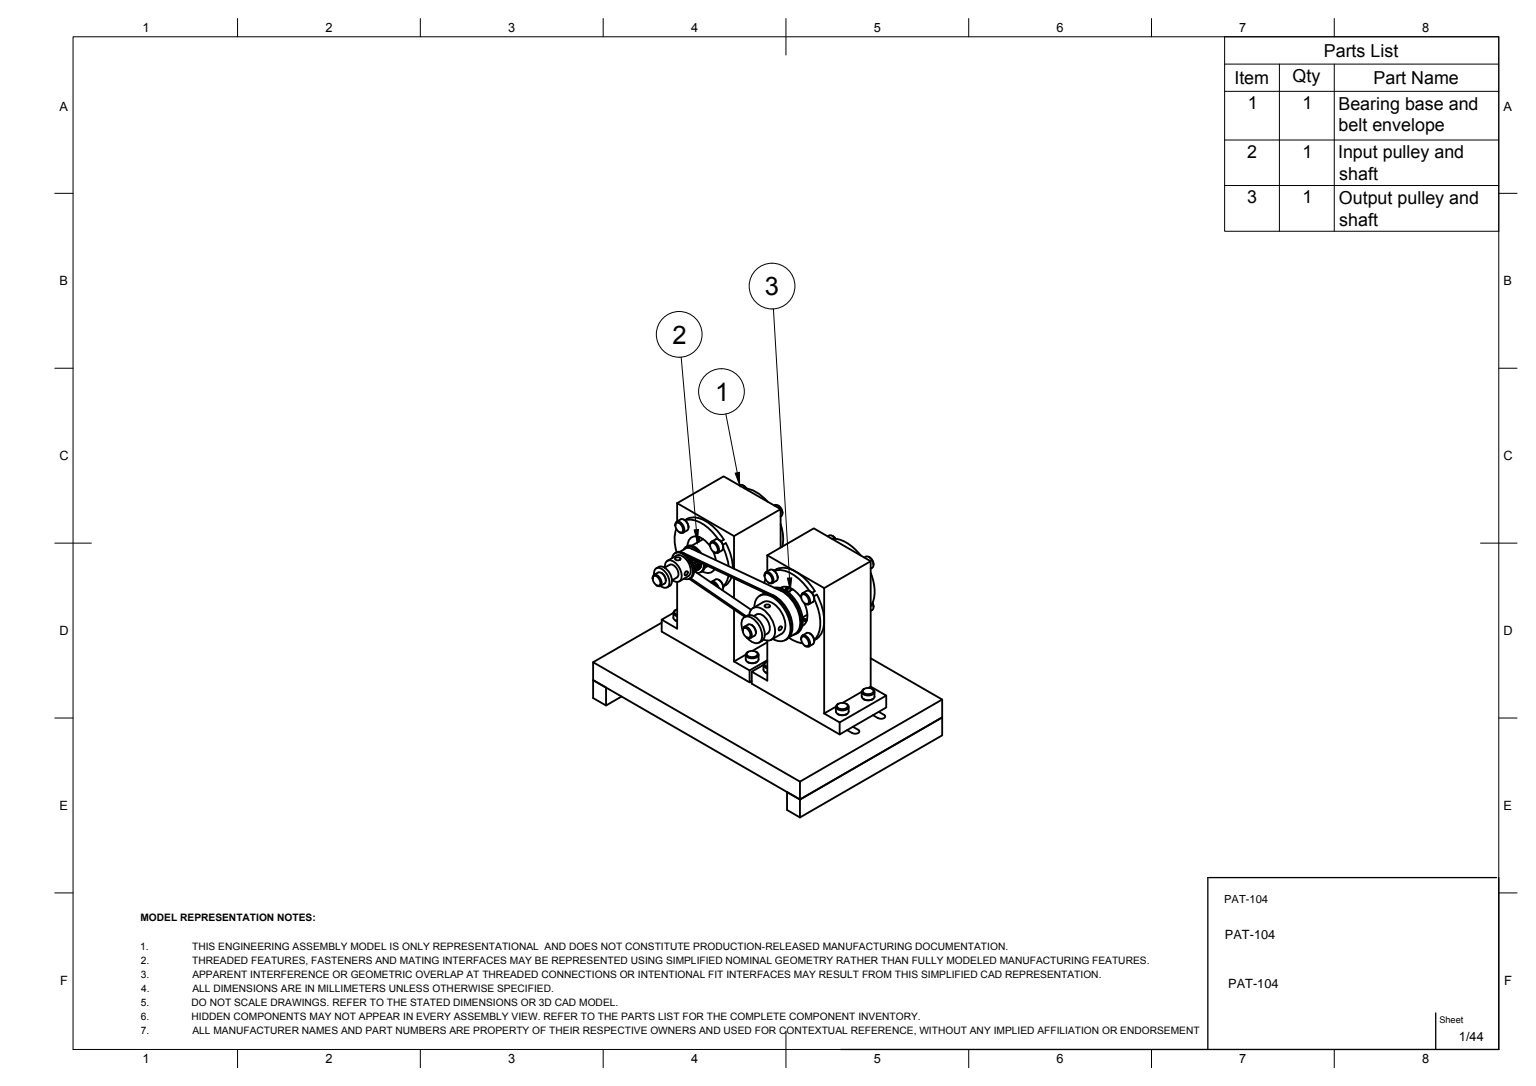
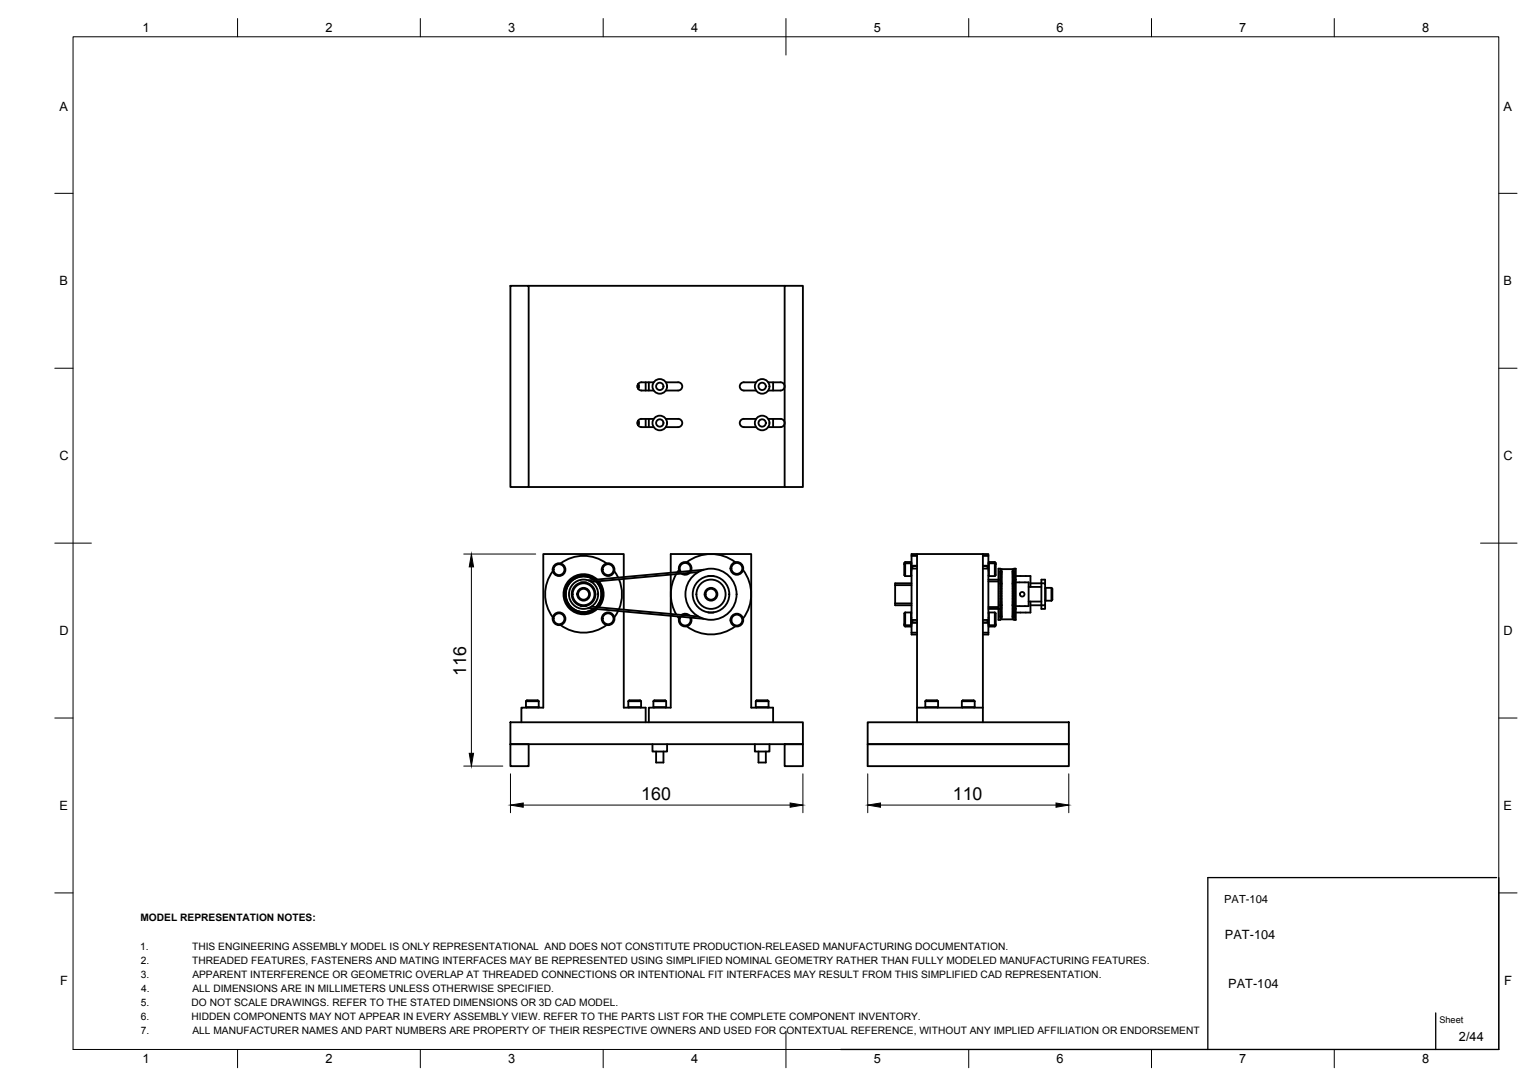
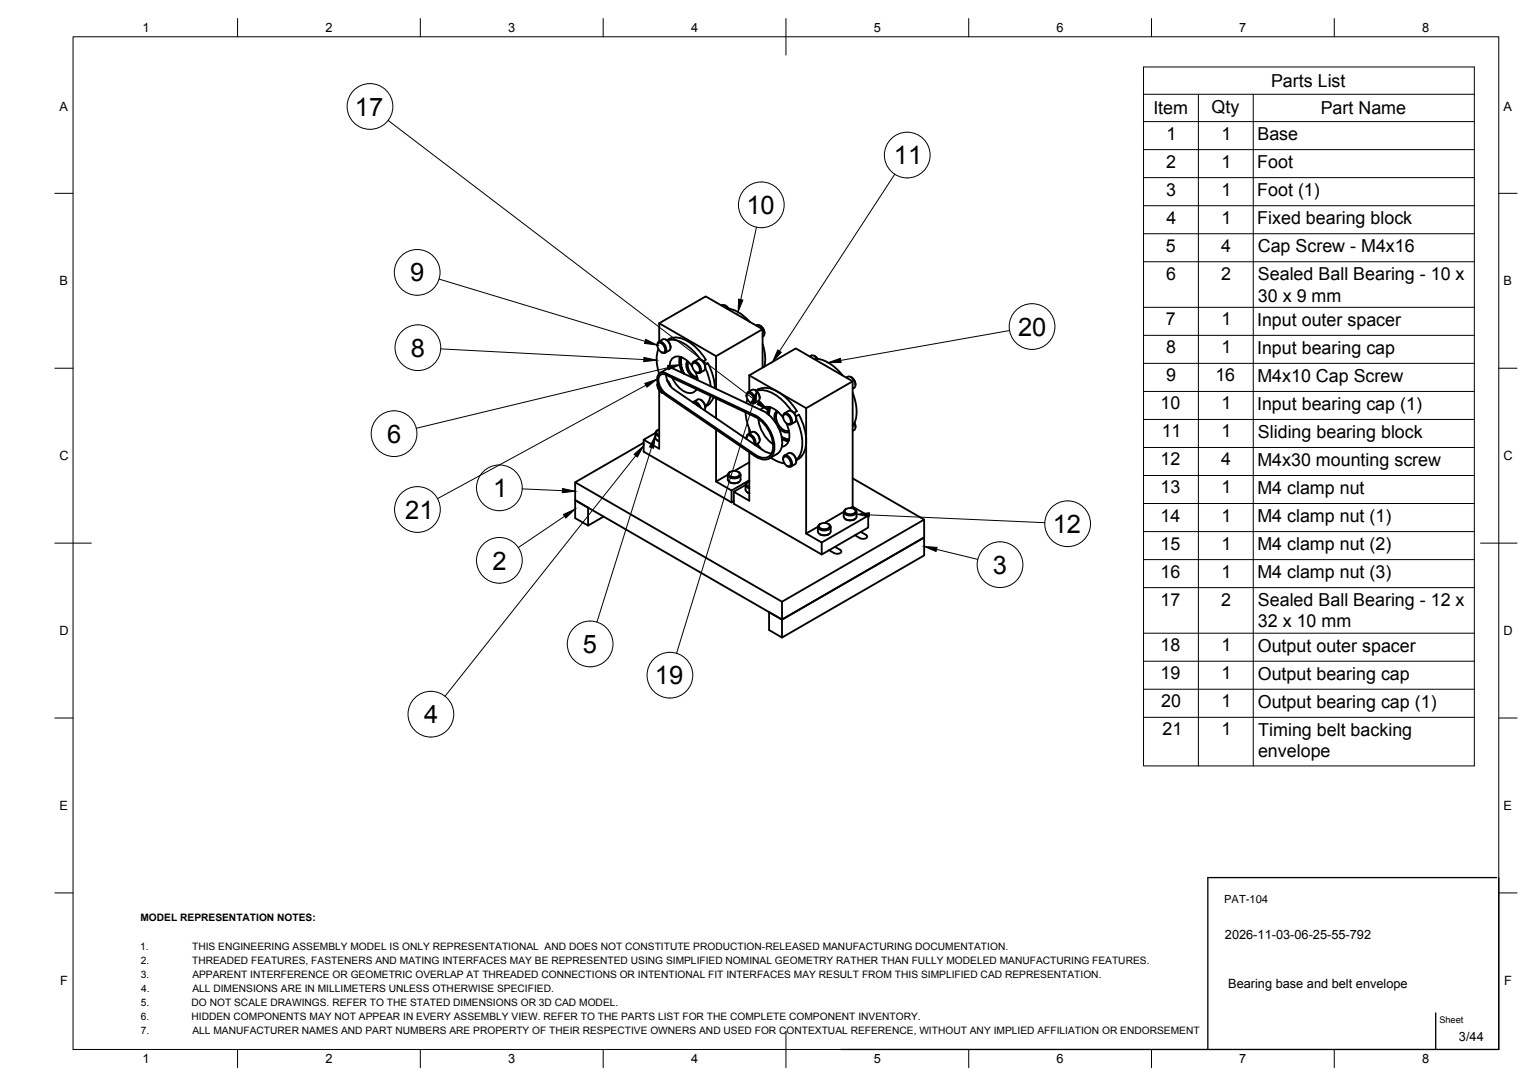
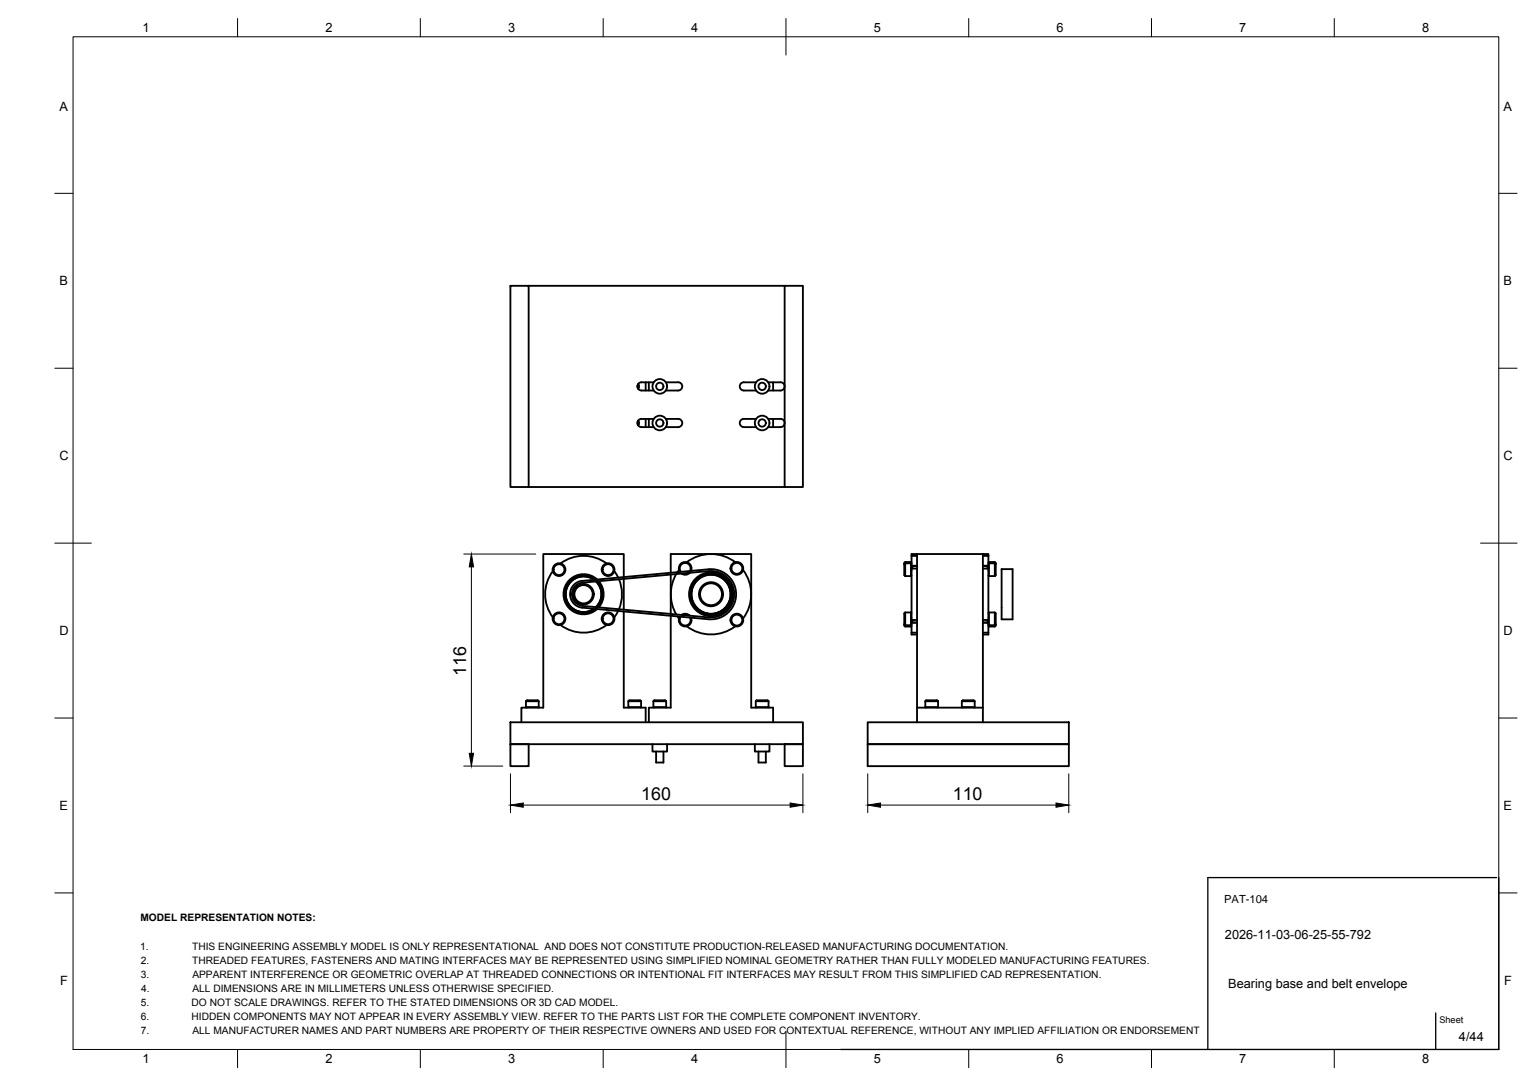
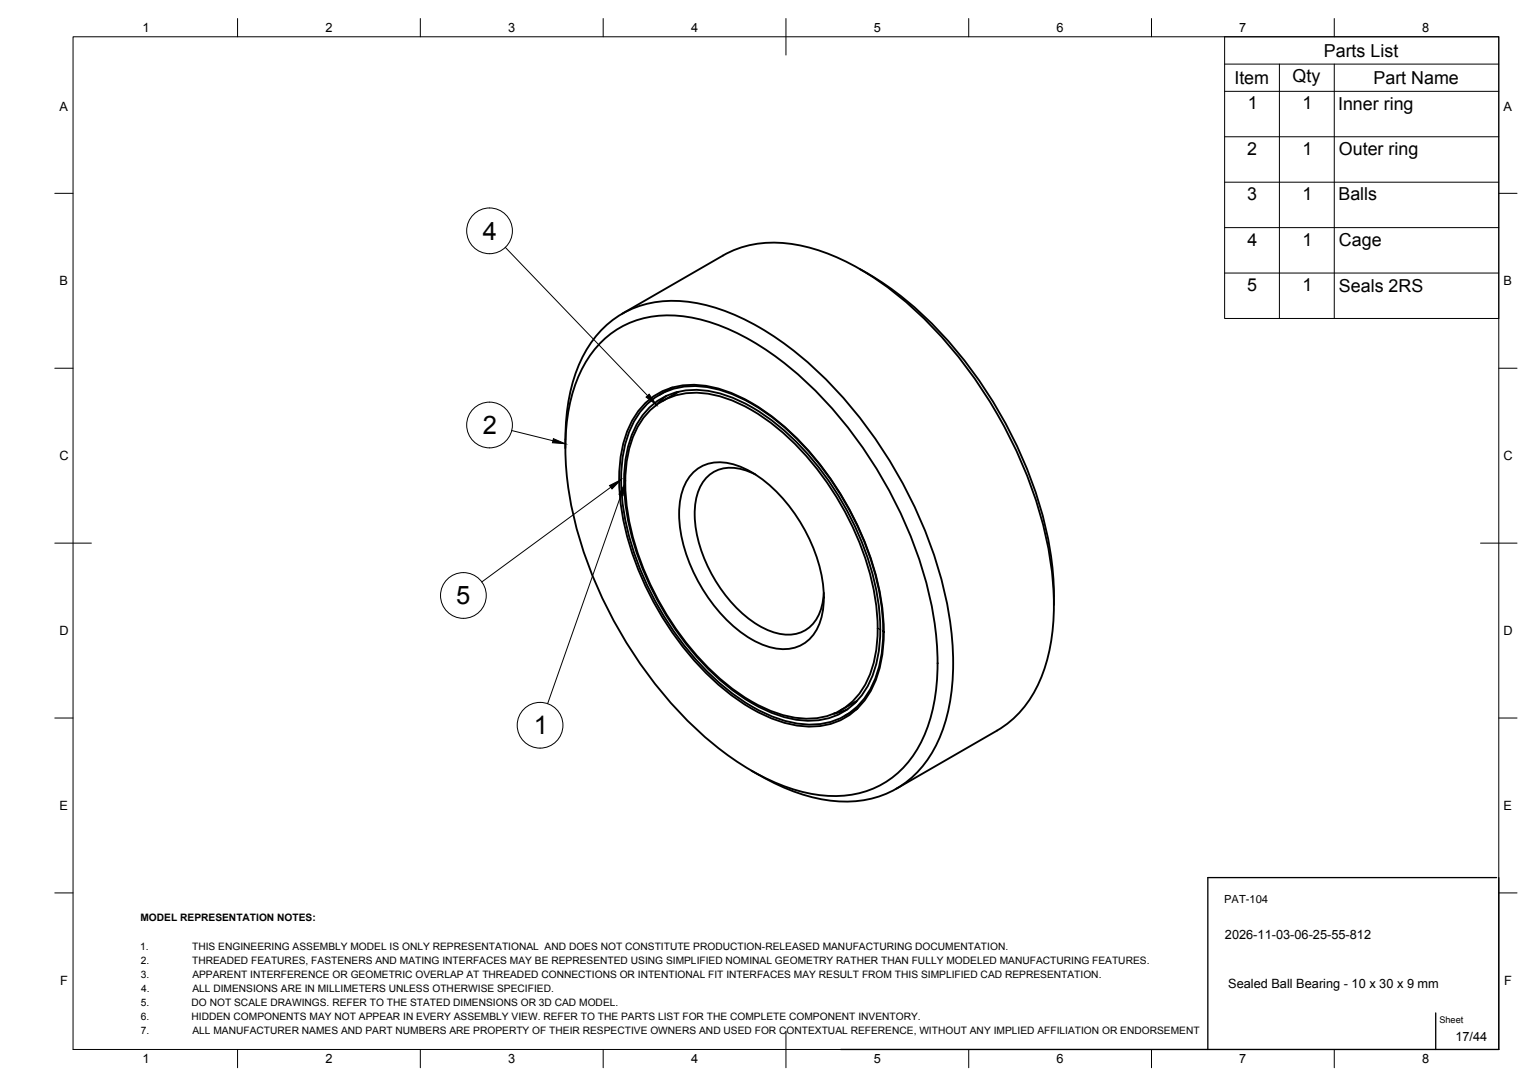
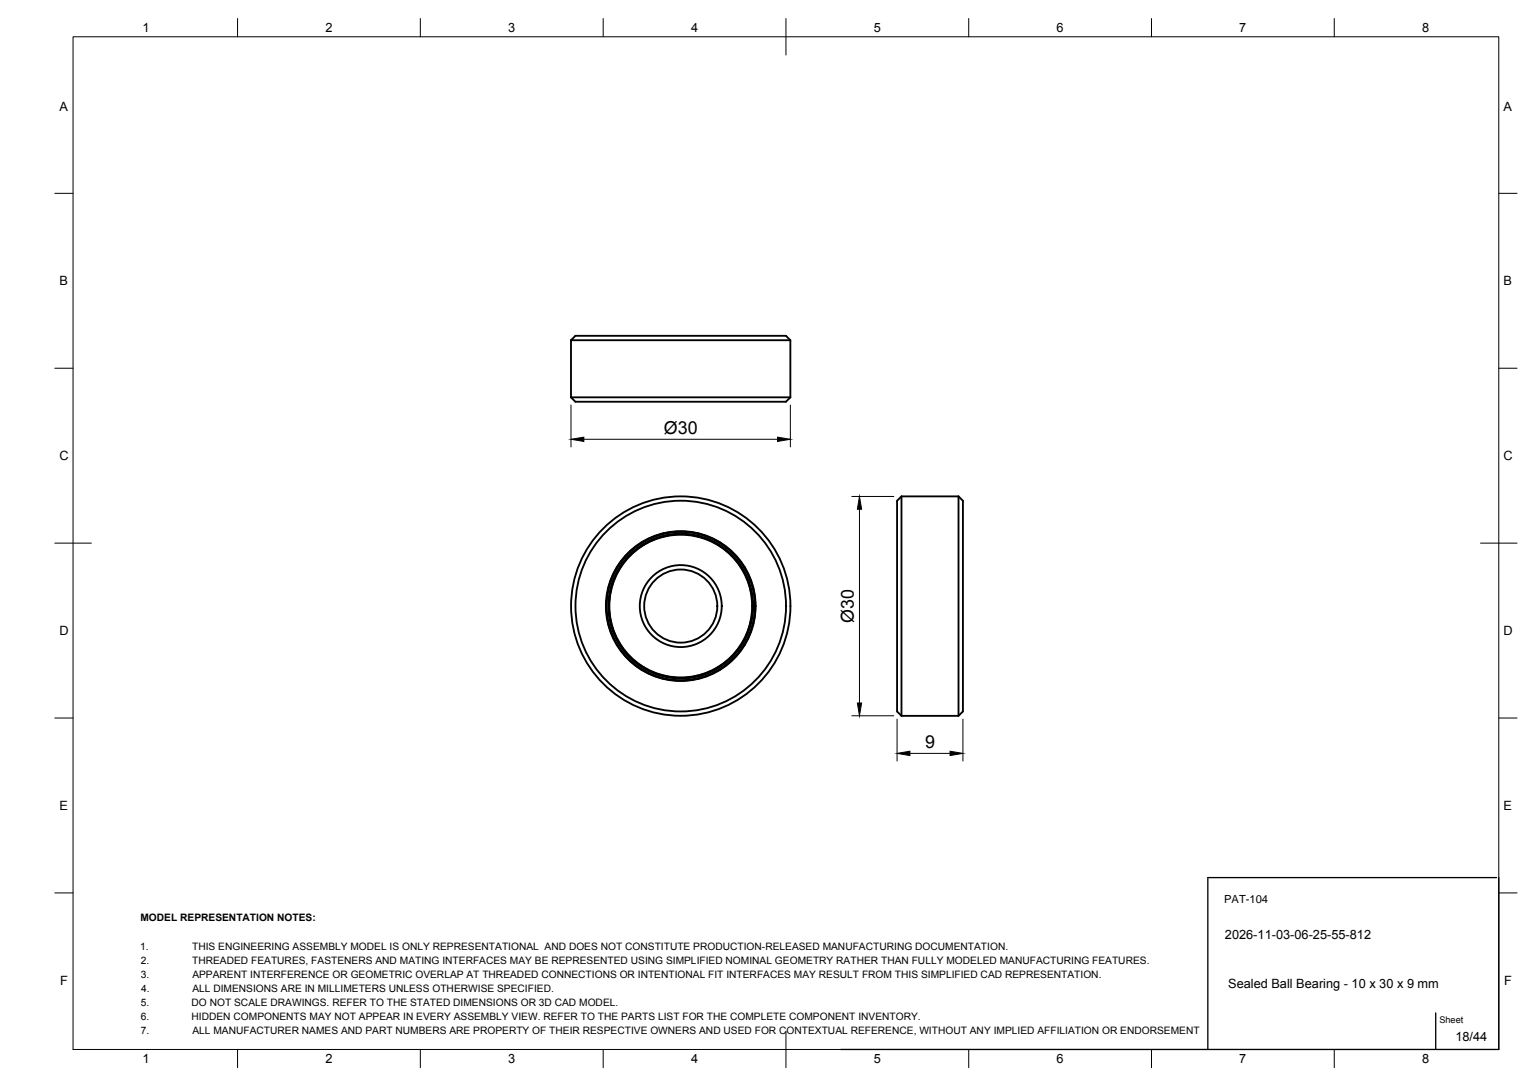
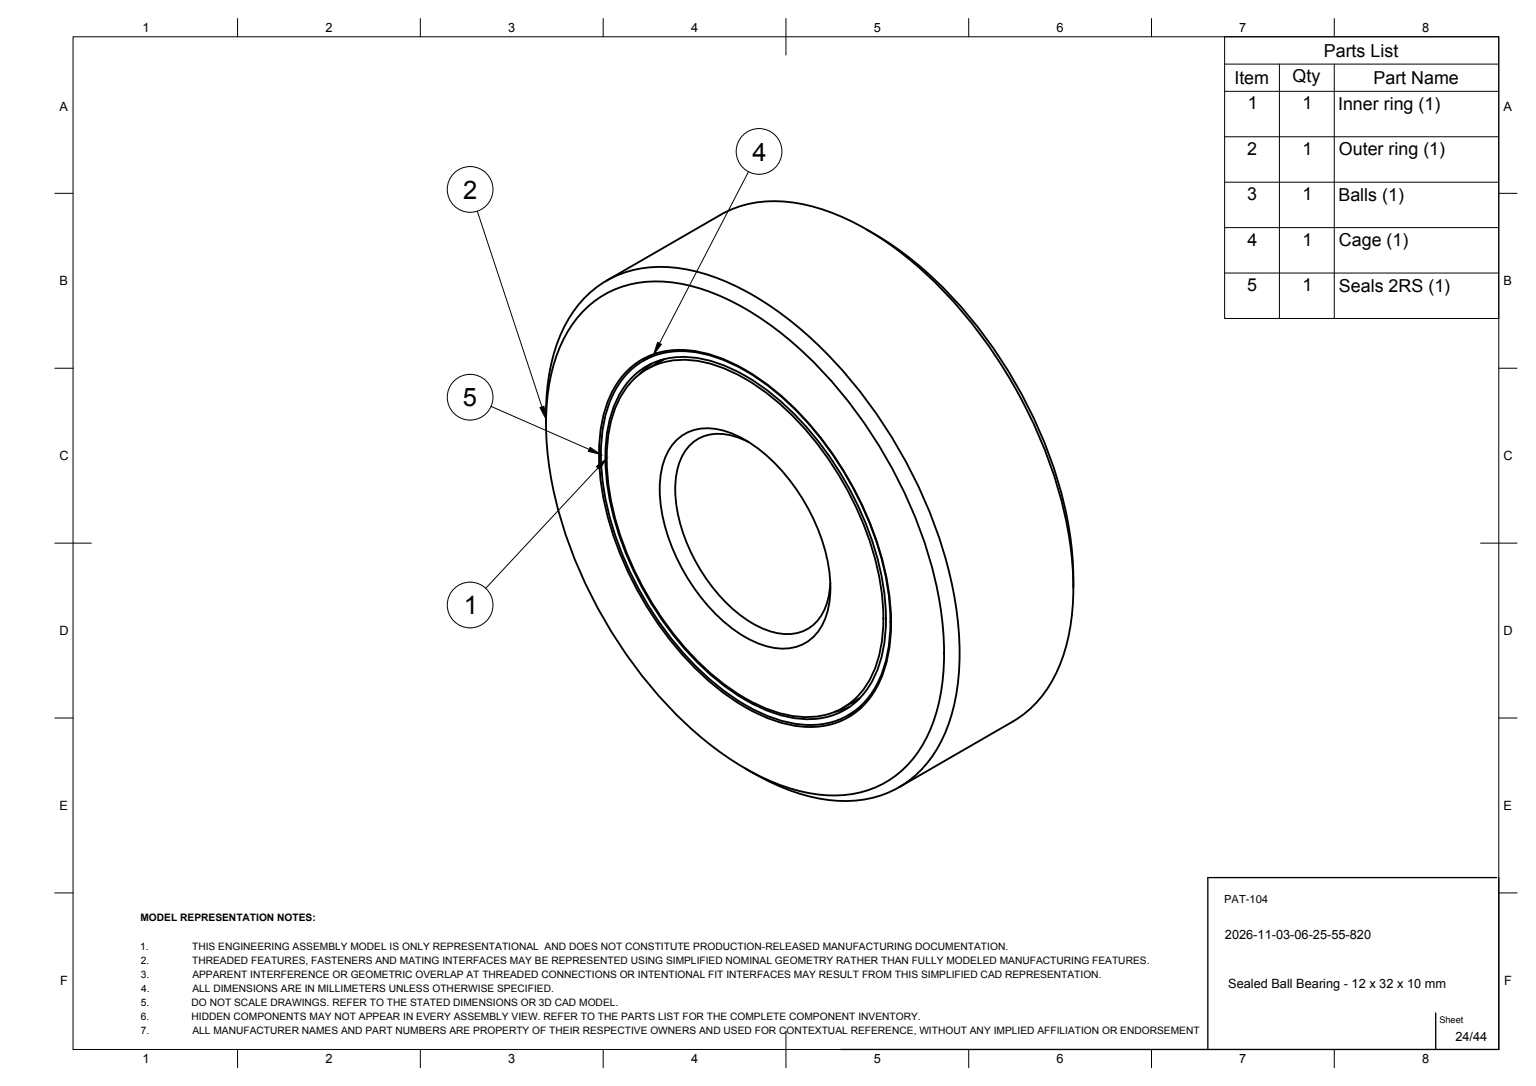
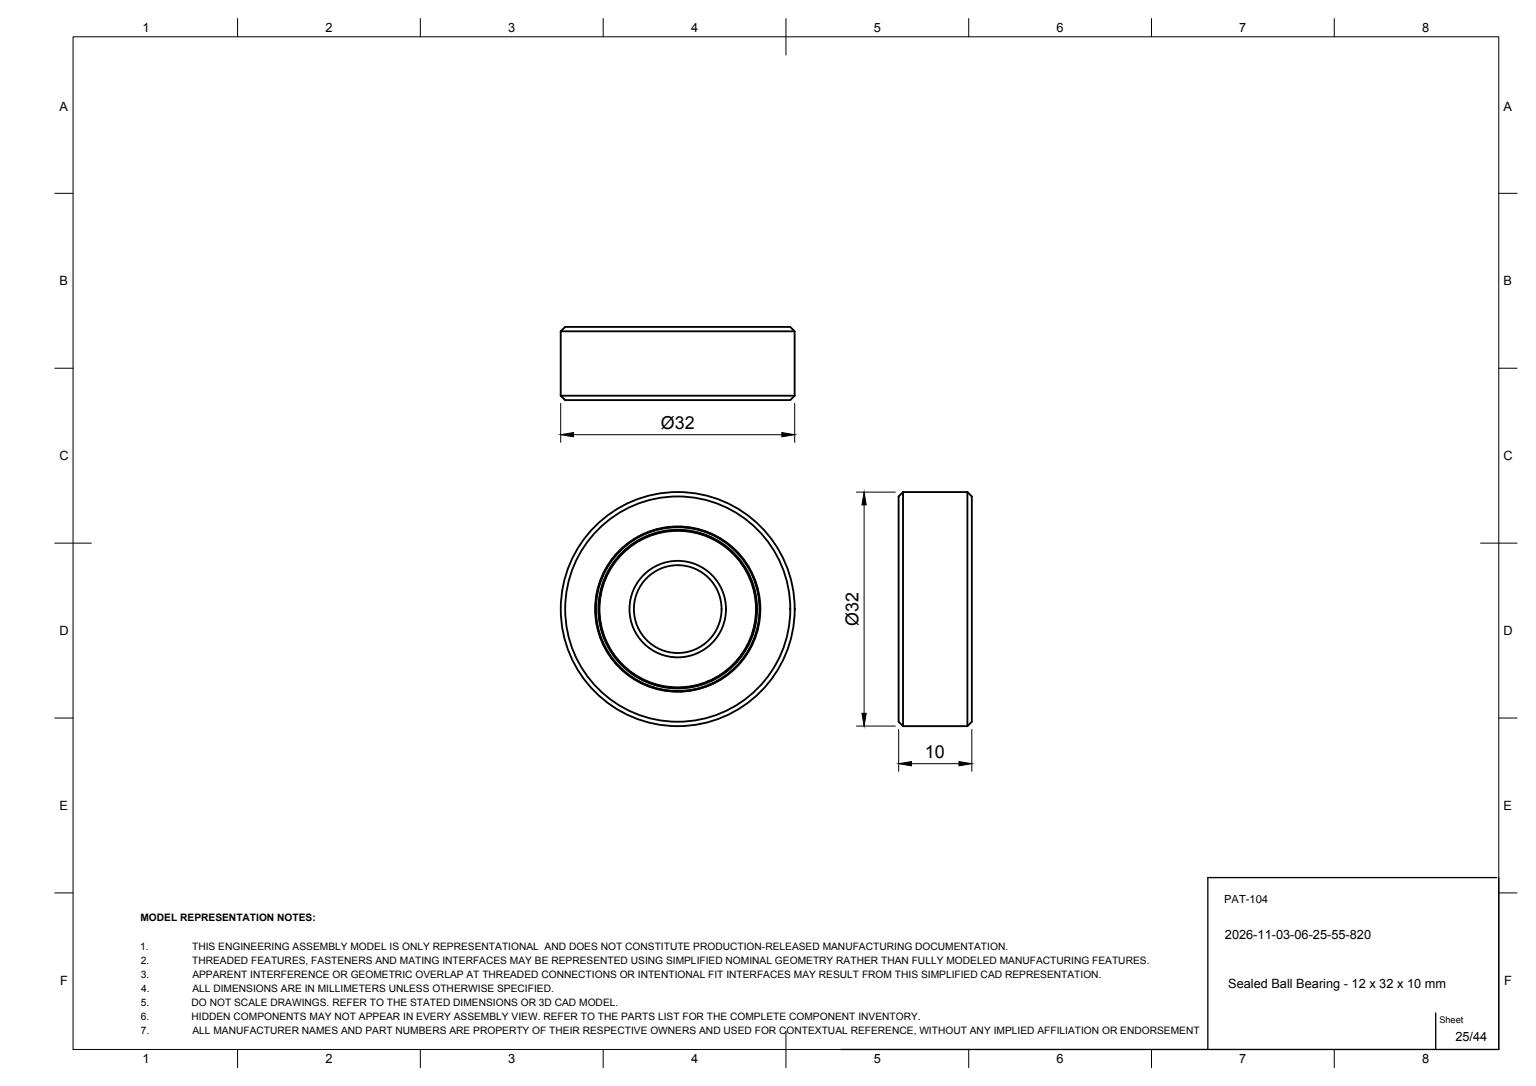
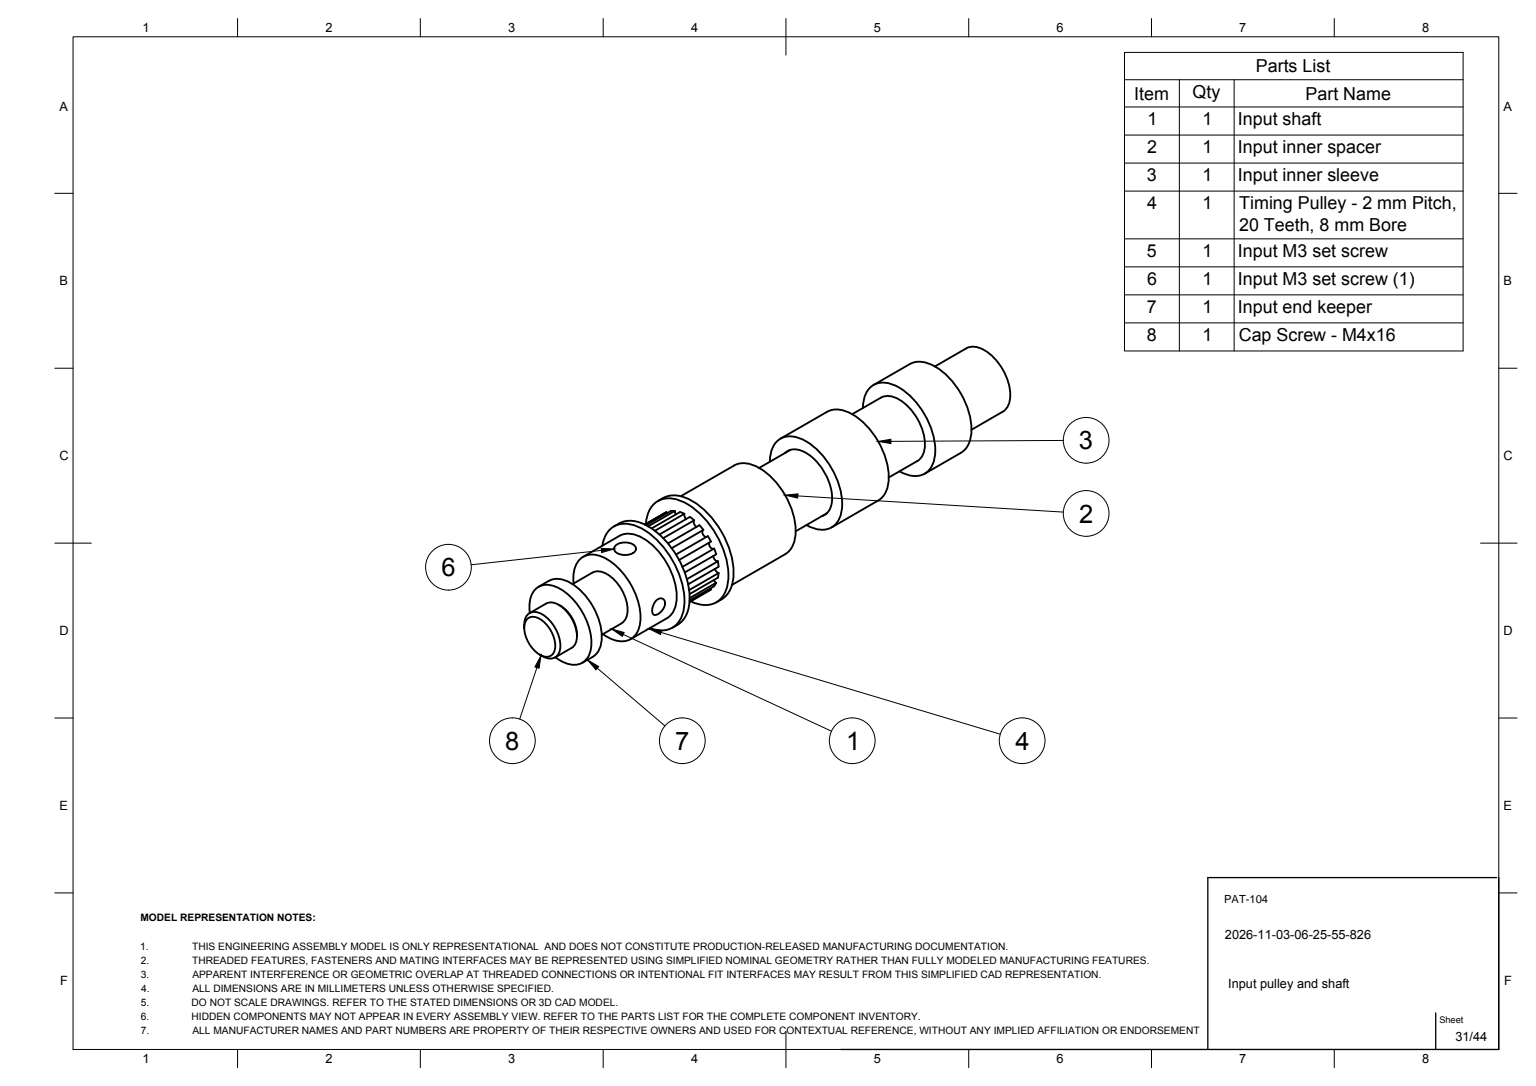
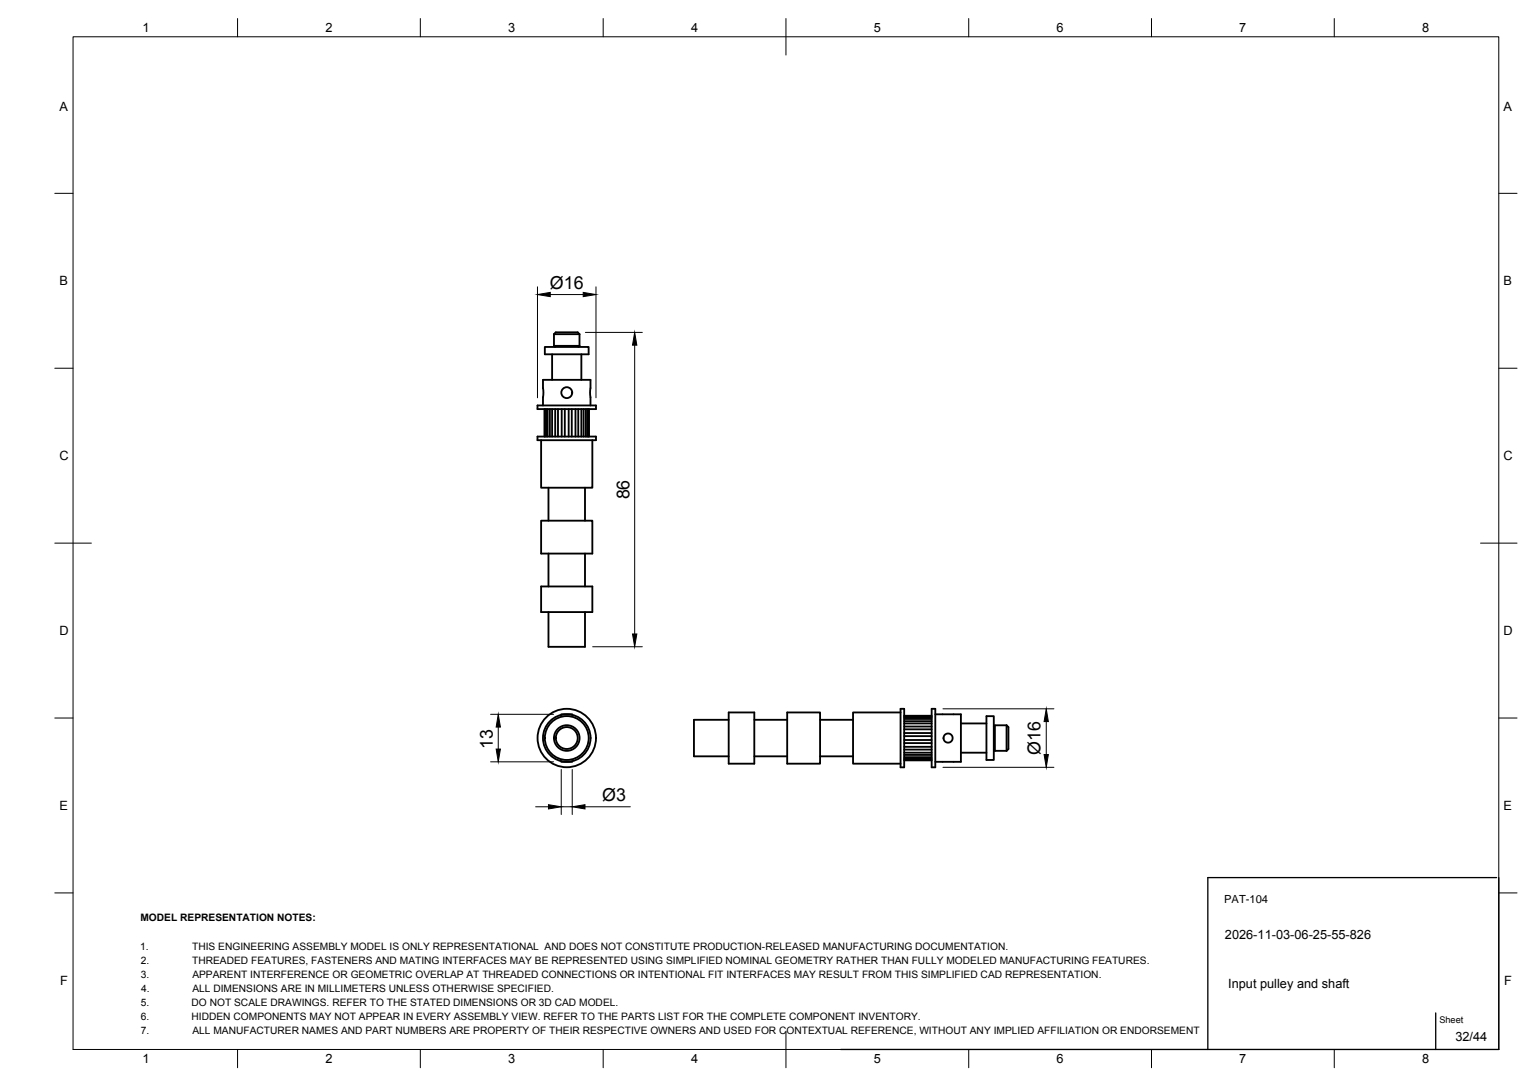
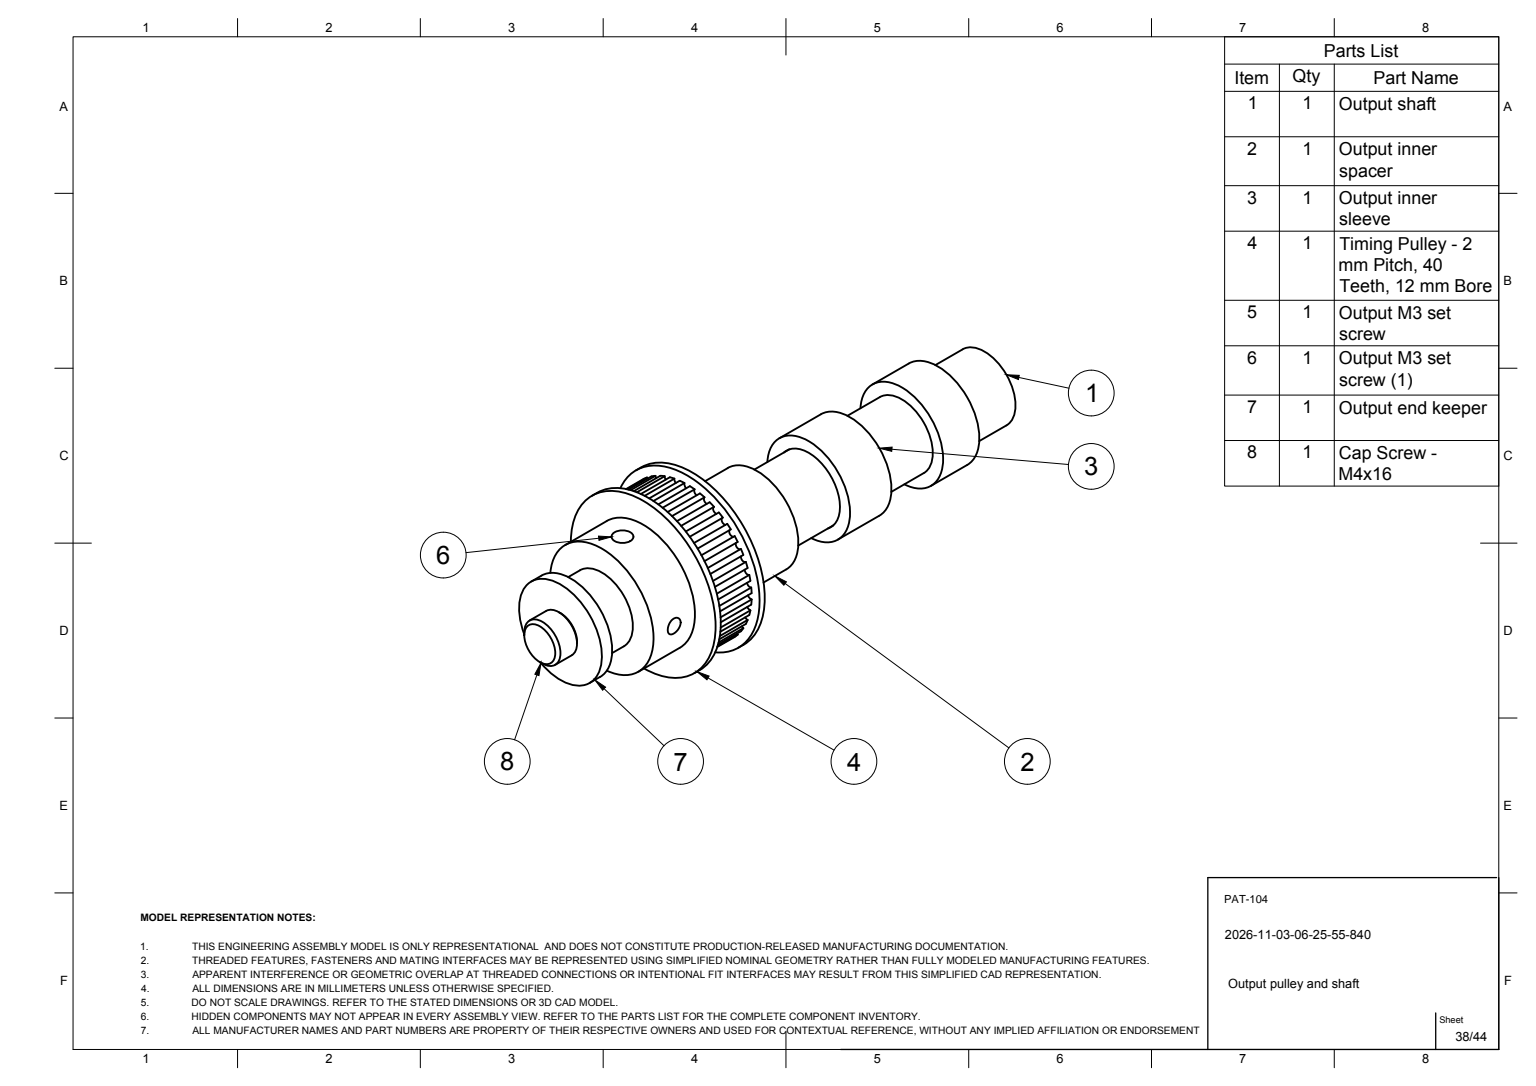
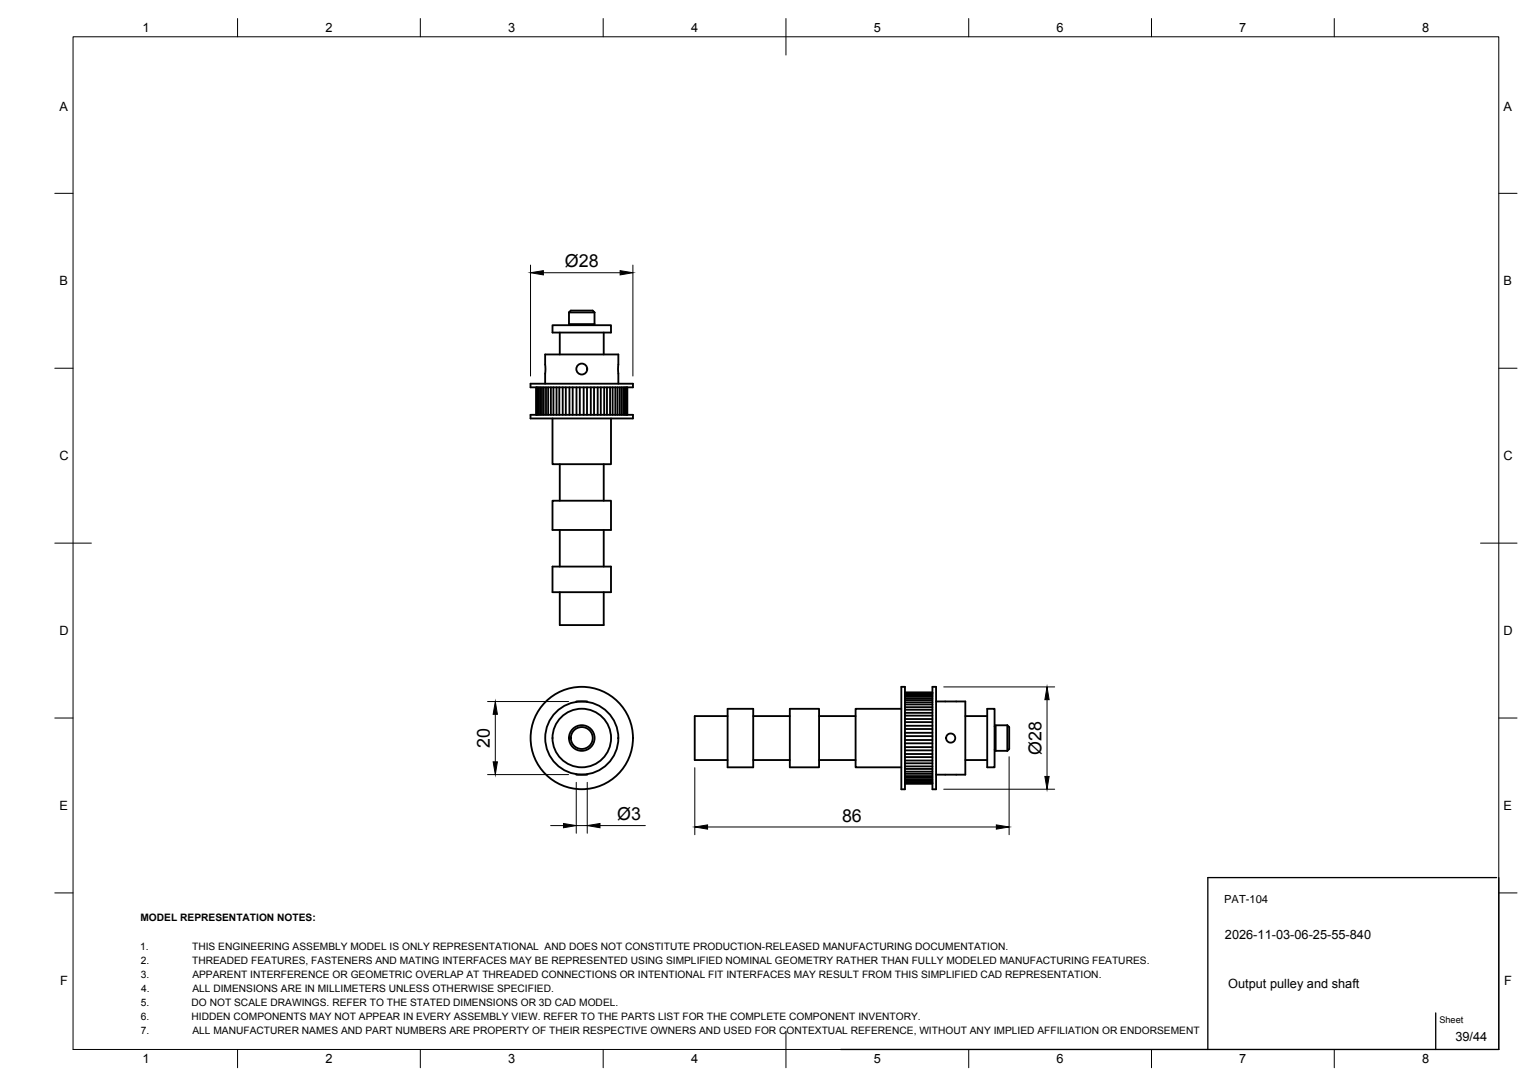
ISO-10303-21;
HEADER;
/* Generated by software containing ST-Developer
 * from STEP Tools, Inc. (www.steptools.com) 
 */

FILE_DESCRIPTION(
/* description */ ('Timing belt drive module 2 mm Pitch Timing 20T-40T'),

/* implementation_level */ '2;1');

FILE_NAME(
/* name */ 'PAT-104',
/* time_stamp */ '2026-10-28T03:25:12-07:00',
/* author */ (''),
/* organization */ (''),
/* preprocessor_version */ 'ST-DEVELOPER v20.2',
/* originating_system */ 'Autodesk Translation Framework v15.17.0.0',
/* authorisation */ '');

FILE_SCHEMA (('AUTOMOTIVE_DESIGN { 1 0 10303 214 3 1 1 }'));
ENDSEC;

DATA;
#10=MECHANICAL_DESIGN_GEOMETRIC_PRESENTATION_REPRESENTATION('',(#524,#525,
#526,#527,#528,#529,#530,#531,#532,#533,#534,#535,#536,#537,#538,#539,#540,
#541,#542,#543,#544,#545,#546,#547,#548,#549,#550,#551,#552,#553,#554,#555,
#556,#557,#558,#559,#560,#561,#562,#563,#564,#565,#566,#567,#568,#569,#570,
#571,#572,#573,#574,#575,#576,#577,#578,#579,#580,#581),#17830);
#11=ORIENTED_CLOSED_SHELL('',*,#9010,.F.);
#12=ORIENTED_CLOSED_SHELL('',*,#9024,.F.);
#13=ORIENTED_CLOSED_SHELL('',*,#9041,.F.);
#14=BREP_WITH_VOIDS('Body1',#9011,(#11));
#15=BREP_WITH_VOIDS('Body1',#9025,(#12));
#16=BREP_WITH_VOIDS('Body1',#9040,(#13));
#17=ITEM_DEFINED_TRANSFORMATION($,$,#9877,#10005);
#18=ITEM_DEFINED_TRANSFORMATION($,$,#9897,#10006);
#19=ITEM_DEFINED_TRANSFORMATION($,$,#9917,#10007);
#20=ITEM_DEFINED_TRANSFORMATION($,$,#9934,#10008);
#21=ITEM_DEFINED_TRANSFORMATION($,$,#9988,#10009);
#22=ITEM_DEFINED_TRANSFORMATION($,$,#10041,#10163);
#23=ITEM_DEFINED_TRANSFORMATION($,$,#10061,#10164);
#24=ITEM_DEFINED_TRANSFORMATION($,$,#10081,#10165);
#25=ITEM_DEFINED_TRANSFORMATION($,$,#10096,#10166);
#26=ITEM_DEFINED_TRANSFORMATION($,$,#10146,#10167);
#27=ITEM_DEFINED_TRANSFORMATION($,$,#9518,#10746);
#28=ITEM_DEFINED_TRANSFORMATION($,$,#9577,#10747);
#29=ITEM_DEFINED_TRANSFORMATION($,$,#9584,#10748);
#30=ITEM_DEFINED_TRANSFORMATION($,$,#9591,#10749);
#31=ITEM_DEFINED_TRANSFORMATION($,$,#9629,#10750);
#32=ITEM_DEFINED_TRANSFORMATION($,$,#9638,#10751);
#33=ITEM_DEFINED_TRANSFORMATION($,$,#9672,#10752);
#34=ITEM_DEFINED_TRANSFORMATION($,$,#9706,#10753);
#35=ITEM_DEFINED_TRANSFORMATION($,$,#9744,#10754);
#36=ITEM_DEFINED_TRANSFORMATION($,$,#9753,#10755);
#37=ITEM_DEFINED_TRANSFORMATION($,$,#9762,#10756);
#38=ITEM_DEFINED_TRANSFORMATION($,$,#9771,#10757);
#39=ITEM_DEFINED_TRANSFORMATION($,$,#9780,#10758);
#40=ITEM_DEFINED_TRANSFORMATION($,$,#9789,#10759);
#41=ITEM_DEFINED_TRANSFORMATION($,$,#9823,#10760);
#42=ITEM_DEFINED_TRANSFORMATION($,$,#9857,#10761);
#43=ITEM_DEFINED_TRANSFORMATION($,$,#10720,#10762);
#44=ITEM_DEFINED_TRANSFORMATION($,$,#10720,#10763);
#45=ITEM_DEFINED_TRANSFORMATION($,$,#10720,#10764);
#46=ITEM_DEFINED_TRANSFORMATION($,$,#10720,#10765);
#47=ITEM_DEFINED_TRANSFORMATION($,$,#9876,#10766);
#48=ITEM_DEFINED_TRANSFORMATION($,$,#9876,#10767);
#49=ITEM_DEFINED_TRANSFORMATION($,$,#10168,#10768);
#50=ITEM_DEFINED_TRANSFORMATION($,$,#10168,#10769);
#51=ITEM_DEFINED_TRANSFORMATION($,$,#10168,#10770);
#52=ITEM_DEFINED_TRANSFORMATION($,$,#10168,#10771);
#53=ITEM_DEFINED_TRANSFORMATION($,$,#10168,#10772);
#54=ITEM_DEFINED_TRANSFORMATION($,$,#10168,#10773);
#55=ITEM_DEFINED_TRANSFORMATION($,$,#10168,#10774);
#56=ITEM_DEFINED_TRANSFORMATION($,$,#10168,#10775);
#57=ITEM_DEFINED_TRANSFORMATION($,$,#10010,#10776);
#58=ITEM_DEFINED_TRANSFORMATION($,$,#10010,#10777);
#59=ITEM_DEFINED_TRANSFORMATION($,$,#10010,#10778);
#60=ITEM_DEFINED_TRANSFORMATION($,$,#10010,#10779);
#61=ITEM_DEFINED_TRANSFORMATION($,$,#10040,#10780);
#62=ITEM_DEFINED_TRANSFORMATION($,$,#10040,#10781);
#63=ITEM_DEFINED_TRANSFORMATION($,$,#10168,#10782);
#64=ITEM_DEFINED_TRANSFORMATION($,$,#10168,#10783);
#65=ITEM_DEFINED_TRANSFORMATION($,$,#10168,#10784);
#66=ITEM_DEFINED_TRANSFORMATION($,$,#10168,#10785);
#67=ITEM_DEFINED_TRANSFORMATION($,$,#10168,#10786);
#68=ITEM_DEFINED_TRANSFORMATION($,$,#10168,#10787);
#69=ITEM_DEFINED_TRANSFORMATION($,$,#10168,#10788);
#70=ITEM_DEFINED_TRANSFORMATION($,$,#10168,#10789);
#71=ITEM_DEFINED_TRANSFORMATION($,$,#10193,#10790);
#72=ITEM_DEFINED_TRANSFORMATION($,$,#10215,#10791);
#73=ITEM_DEFINED_TRANSFORMATION($,$,#10228,#10792);
#74=ITEM_DEFINED_TRANSFORMATION($,$,#10237,#10793);
#75=ITEM_DEFINED_TRANSFORMATION($,$,#10243,#10794);
#76=ITEM_DEFINED_TRANSFORMATION($,$,#10249,#10795);
#77=ITEM_DEFINED_TRANSFORMATION($,$,#10258,#10796);
#78=ITEM_DEFINED_TRANSFORMATION($,$,#10720,#10797);
#79=ITEM_DEFINED_TRANSFORMATION($,$,#10401,#10798);
#80=ITEM_DEFINED_TRANSFORMATION($,$,#10419,#10799);
#81=ITEM_DEFINED_TRANSFORMATION($,$,#10428,#10800);
#82=ITEM_DEFINED_TRANSFORMATION($,$,#10437,#10801);
#83=ITEM_DEFINED_TRANSFORMATION($,$,#10443,#10802);
#84=ITEM_DEFINED_TRANSFORMATION($,$,#10449,#10803);
#85=ITEM_DEFINED_TRANSFORMATION($,$,#10458,#10804);
#86=ITEM_DEFINED_TRANSFORMATION($,$,#10720,#10805);
#87=ITEM_DEFINED_TRANSFORMATION($,$,#9517,#10806);
#88=ITEM_DEFINED_TRANSFORMATION($,$,#10192,#10807);
#89=ITEM_DEFINED_TRANSFORMATION($,$,#10400,#10808);
#90=(
REPRESENTATION_RELATIONSHIP($,$,#18025,#18024)
REPRESENTATION_RELATIONSHIP_WITH_TRANSFORMATION(#17)
SHAPE_REPRESENTATION_RELATIONSHIP()
);
#91=(
REPRESENTATION_RELATIONSHIP($,$,#18026,#18024)
REPRESENTATION_RELATIONSHIP_WITH_TRANSFORMATION(#18)
SHAPE_REPRESENTATION_RELATIONSHIP()
);
#92=(
REPRESENTATION_RELATIONSHIP($,$,#18027,#18024)
REPRESENTATION_RELATIONSHIP_WITH_TRANSFORMATION(#19)
SHAPE_REPRESENTATION_RELATIONSHIP()
);
#93=(
REPRESENTATION_RELATIONSHIP($,$,#18028,#18024)
REPRESENTATION_RELATIONSHIP_WITH_TRANSFORMATION(#20)
SHAPE_REPRESENTATION_RELATIONSHIP()
);
#94=(
REPRESENTATION_RELATIONSHIP($,$,#18029,#18024)
REPRESENTATION_RELATIONSHIP_WITH_TRANSFORMATION(#21)
SHAPE_REPRESENTATION_RELATIONSHIP()
);
#95=(
REPRESENTATION_RELATIONSHIP($,$,#18032,#18031)
REPRESENTATION_RELATIONSHIP_WITH_TRANSFORMATION(#22)
SHAPE_REPRESENTATION_RELATIONSHIP()
);
#96=(
REPRESENTATION_RELATIONSHIP($,$,#18033,#18031)
REPRESENTATION_RELATIONSHIP_WITH_TRANSFORMATION(#23)
SHAPE_REPRESENTATION_RELATIONSHIP()
);
#97=(
REPRESENTATION_RELATIONSHIP($,$,#18034,#18031)
REPRESENTATION_RELATIONSHIP_WITH_TRANSFORMATION(#24)
SHAPE_REPRESENTATION_RELATIONSHIP()
);
#98=(
REPRESENTATION_RELATIONSHIP($,$,#18035,#18031)
REPRESENTATION_RELATIONSHIP_WITH_TRANSFORMATION(#25)
SHAPE_REPRESENTATION_RELATIONSHIP()
);
#99=(
REPRESENTATION_RELATIONSHIP($,$,#18036,#18031)
REPRESENTATION_RELATIONSHIP_WITH_TRANSFORMATION(#26)
SHAPE_REPRESENTATION_RELATIONSHIP()
);
#100=(
REPRESENTATION_RELATIONSHIP($,$,#18008,#18007)
REPRESENTATION_RELATIONSHIP_WITH_TRANSFORMATION(#27)
SHAPE_REPRESENTATION_RELATIONSHIP()
);
#101=(
REPRESENTATION_RELATIONSHIP($,$,#18009,#18007)
REPRESENTATION_RELATIONSHIP_WITH_TRANSFORMATION(#28)
SHAPE_REPRESENTATION_RELATIONSHIP()
);
#102=(
REPRESENTATION_RELATIONSHIP($,$,#18010,#18007)
REPRESENTATION_RELATIONSHIP_WITH_TRANSFORMATION(#29)
SHAPE_REPRESENTATION_RELATIONSHIP()
);
#103=(
REPRESENTATION_RELATIONSHIP($,$,#18011,#18007)
REPRESENTATION_RELATIONSHIP_WITH_TRANSFORMATION(#30)
SHAPE_REPRESENTATION_RELATIONSHIP()
);
#104=(
REPRESENTATION_RELATIONSHIP($,$,#18012,#18007)
REPRESENTATION_RELATIONSHIP_WITH_TRANSFORMATION(#31)
SHAPE_REPRESENTATION_RELATIONSHIP()
);
#105=(
REPRESENTATION_RELATIONSHIP($,$,#18013,#18007)
REPRESENTATION_RELATIONSHIP_WITH_TRANSFORMATION(#32)
SHAPE_REPRESENTATION_RELATIONSHIP()
);
#106=(
REPRESENTATION_RELATIONSHIP($,$,#18014,#18007)
REPRESENTATION_RELATIONSHIP_WITH_TRANSFORMATION(#33)
SHAPE_REPRESENTATION_RELATIONSHIP()
);
#107=(
REPRESENTATION_RELATIONSHIP($,$,#18015,#18007)
REPRESENTATION_RELATIONSHIP_WITH_TRANSFORMATION(#34)
SHAPE_REPRESENTATION_RELATIONSHIP()
);
#108=(
REPRESENTATION_RELATIONSHIP($,$,#18016,#18007)
REPRESENTATION_RELATIONSHIP_WITH_TRANSFORMATION(#35)
SHAPE_REPRESENTATION_RELATIONSHIP()
);
#109=(
REPRESENTATION_RELATIONSHIP($,$,#18017,#18007)
REPRESENTATION_RELATIONSHIP_WITH_TRANSFORMATION(#36)
SHAPE_REPRESENTATION_RELATIONSHIP()
);
#110=(
REPRESENTATION_RELATIONSHIP($,$,#18018,#18007)
REPRESENTATION_RELATIONSHIP_WITH_TRANSFORMATION(#37)
SHAPE_REPRESENTATION_RELATIONSHIP()
);
#111=(
REPRESENTATION_RELATIONSHIP($,$,#18019,#18007)
REPRESENTATION_RELATIONSHIP_WITH_TRANSFORMATION(#38)
SHAPE_REPRESENTATION_RELATIONSHIP()
);
#112=(
REPRESENTATION_RELATIONSHIP($,$,#18020,#18007)
REPRESENTATION_RELATIONSHIP_WITH_TRANSFORMATION(#39)
SHAPE_REPRESENTATION_RELATIONSHIP()
);
#113=(
REPRESENTATION_RELATIONSHIP($,$,#18021,#18007)
REPRESENTATION_RELATIONSHIP_WITH_TRANSFORMATION(#40)
SHAPE_REPRESENTATION_RELATIONSHIP()
);
#114=(
REPRESENTATION_RELATIONSHIP($,$,#18022,#18007)
REPRESENTATION_RELATIONSHIP_WITH_TRANSFORMATION(#41)
SHAPE_REPRESENTATION_RELATIONSHIP()
);
#115=(
REPRESENTATION_RELATIONSHIP($,$,#18023,#18007)
REPRESENTATION_RELATIONSHIP_WITH_TRANSFORMATION(#42)
SHAPE_REPRESENTATION_RELATIONSHIP()
);
#116=(
REPRESENTATION_RELATIONSHIP($,$,#18054,#18007)
REPRESENTATION_RELATIONSHIP_WITH_TRANSFORMATION(#43)
SHAPE_REPRESENTATION_RELATIONSHIP()
);
#117=(
REPRESENTATION_RELATIONSHIP($,$,#18054,#18007)
REPRESENTATION_RELATIONSHIP_WITH_TRANSFORMATION(#44)
SHAPE_REPRESENTATION_RELATIONSHIP()
);
#118=(
REPRESENTATION_RELATIONSHIP($,$,#18054,#18007)
REPRESENTATION_RELATIONSHIP_WITH_TRANSFORMATION(#45)
SHAPE_REPRESENTATION_RELATIONSHIP()
);
#119=(
REPRESENTATION_RELATIONSHIP($,$,#18054,#18007)
REPRESENTATION_RELATIONSHIP_WITH_TRANSFORMATION(#46)
SHAPE_REPRESENTATION_RELATIONSHIP()
);
#120=(
REPRESENTATION_RELATIONSHIP($,$,#18024,#18007)
REPRESENTATION_RELATIONSHIP_WITH_TRANSFORMATION(#47)
SHAPE_REPRESENTATION_RELATIONSHIP()
);
#121=(
REPRESENTATION_RELATIONSHIP($,$,#18024,#18007)
REPRESENTATION_RELATIONSHIP_WITH_TRANSFORMATION(#48)
SHAPE_REPRESENTATION_RELATIONSHIP()
);
#122=(
REPRESENTATION_RELATIONSHIP($,$,#18037,#18007)
REPRESENTATION_RELATIONSHIP_WITH_TRANSFORMATION(#49)
SHAPE_REPRESENTATION_RELATIONSHIP()
);
#123=(
REPRESENTATION_RELATIONSHIP($,$,#18037,#18007)
REPRESENTATION_RELATIONSHIP_WITH_TRANSFORMATION(#50)
SHAPE_REPRESENTATION_RELATIONSHIP()
);
#124=(
REPRESENTATION_RELATIONSHIP($,$,#18037,#18007)
REPRESENTATION_RELATIONSHIP_WITH_TRANSFORMATION(#51)
SHAPE_REPRESENTATION_RELATIONSHIP()
);
#125=(
REPRESENTATION_RELATIONSHIP($,$,#18037,#18007)
REPRESENTATION_RELATIONSHIP_WITH_TRANSFORMATION(#52)
SHAPE_REPRESENTATION_RELATIONSHIP()
);
#126=(
REPRESENTATION_RELATIONSHIP($,$,#18037,#18007)
REPRESENTATION_RELATIONSHIP_WITH_TRANSFORMATION(#53)
SHAPE_REPRESENTATION_RELATIONSHIP()
);
#127=(
REPRESENTATION_RELATIONSHIP($,$,#18037,#18007)
REPRESENTATION_RELATIONSHIP_WITH_TRANSFORMATION(#54)
SHAPE_REPRESENTATION_RELATIONSHIP()
);
#128=(
REPRESENTATION_RELATIONSHIP($,$,#18037,#18007)
REPRESENTATION_RELATIONSHIP_WITH_TRANSFORMATION(#55)
SHAPE_REPRESENTATION_RELATIONSHIP()
);
#129=(
REPRESENTATION_RELATIONSHIP($,$,#18037,#18007)
REPRESENTATION_RELATIONSHIP_WITH_TRANSFORMATION(#56)
SHAPE_REPRESENTATION_RELATIONSHIP()
);
#130=(
REPRESENTATION_RELATIONSHIP($,$,#18030,#18007)
REPRESENTATION_RELATIONSHIP_WITH_TRANSFORMATION(#57)
SHAPE_REPRESENTATION_RELATIONSHIP()
);
#131=(
REPRESENTATION_RELATIONSHIP($,$,#18030,#18007)
REPRESENTATION_RELATIONSHIP_WITH_TRANSFORMATION(#58)
SHAPE_REPRESENTATION_RELATIONSHIP()
);
#132=(
REPRESENTATION_RELATIONSHIP($,$,#18030,#18007)
REPRESENTATION_RELATIONSHIP_WITH_TRANSFORMATION(#59)
SHAPE_REPRESENTATION_RELATIONSHIP()
);
#133=(
REPRESENTATION_RELATIONSHIP($,$,#18030,#18007)
REPRESENTATION_RELATIONSHIP_WITH_TRANSFORMATION(#60)
SHAPE_REPRESENTATION_RELATIONSHIP()
);
#134=(
REPRESENTATION_RELATIONSHIP($,$,#18031,#18007)
REPRESENTATION_RELATIONSHIP_WITH_TRANSFORMATION(#61)
SHAPE_REPRESENTATION_RELATIONSHIP()
);
#135=(
REPRESENTATION_RELATIONSHIP($,$,#18031,#18007)
REPRESENTATION_RELATIONSHIP_WITH_TRANSFORMATION(#62)
SHAPE_REPRESENTATION_RELATIONSHIP()
);
#136=(
REPRESENTATION_RELATIONSHIP($,$,#18037,#18007)
REPRESENTATION_RELATIONSHIP_WITH_TRANSFORMATION(#63)
SHAPE_REPRESENTATION_RELATIONSHIP()
);
#137=(
REPRESENTATION_RELATIONSHIP($,$,#18037,#18007)
REPRESENTATION_RELATIONSHIP_WITH_TRANSFORMATION(#64)
SHAPE_REPRESENTATION_RELATIONSHIP()
);
#138=(
REPRESENTATION_RELATIONSHIP($,$,#18037,#18007)
REPRESENTATION_RELATIONSHIP_WITH_TRANSFORMATION(#65)
SHAPE_REPRESENTATION_RELATIONSHIP()
);
#139=(
REPRESENTATION_RELATIONSHIP($,$,#18037,#18007)
REPRESENTATION_RELATIONSHIP_WITH_TRANSFORMATION(#66)
SHAPE_REPRESENTATION_RELATIONSHIP()
);
#140=(
REPRESENTATION_RELATIONSHIP($,$,#18037,#18007)
REPRESENTATION_RELATIONSHIP_WITH_TRANSFORMATION(#67)
SHAPE_REPRESENTATION_RELATIONSHIP()
);
#141=(
REPRESENTATION_RELATIONSHIP($,$,#18037,#18007)
REPRESENTATION_RELATIONSHIP_WITH_TRANSFORMATION(#68)
SHAPE_REPRESENTATION_RELATIONSHIP()
);
#142=(
REPRESENTATION_RELATIONSHIP($,$,#18037,#18007)
REPRESENTATION_RELATIONSHIP_WITH_TRANSFORMATION(#69)
SHAPE_REPRESENTATION_RELATIONSHIP()
);
#143=(
REPRESENTATION_RELATIONSHIP($,$,#18037,#18007)
REPRESENTATION_RELATIONSHIP_WITH_TRANSFORMATION(#70)
SHAPE_REPRESENTATION_RELATIONSHIP()
);
#144=(
REPRESENTATION_RELATIONSHIP($,$,#18039,#18038)
REPRESENTATION_RELATIONSHIP_WITH_TRANSFORMATION(#71)
SHAPE_REPRESENTATION_RELATIONSHIP()
);
#145=(
REPRESENTATION_RELATIONSHIP($,$,#18040,#18038)
REPRESENTATION_RELATIONSHIP_WITH_TRANSFORMATION(#72)
SHAPE_REPRESENTATION_RELATIONSHIP()
);
#146=(
REPRESENTATION_RELATIONSHIP($,$,#18041,#18038)
REPRESENTATION_RELATIONSHIP_WITH_TRANSFORMATION(#73)
SHAPE_REPRESENTATION_RELATIONSHIP()
);
#147=(
REPRESENTATION_RELATIONSHIP($,$,#18042,#18038)
REPRESENTATION_RELATIONSHIP_WITH_TRANSFORMATION(#74)
SHAPE_REPRESENTATION_RELATIONSHIP()
);
#148=(
REPRESENTATION_RELATIONSHIP($,$,#18043,#18038)
REPRESENTATION_RELATIONSHIP_WITH_TRANSFORMATION(#75)
SHAPE_REPRESENTATION_RELATIONSHIP()
);
#149=(
REPRESENTATION_RELATIONSHIP($,$,#18044,#18038)
REPRESENTATION_RELATIONSHIP_WITH_TRANSFORMATION(#76)
SHAPE_REPRESENTATION_RELATIONSHIP()
);
#150=(
REPRESENTATION_RELATIONSHIP($,$,#18045,#18038)
REPRESENTATION_RELATIONSHIP_WITH_TRANSFORMATION(#77)
SHAPE_REPRESENTATION_RELATIONSHIP()
);
#151=(
REPRESENTATION_RELATIONSHIP($,$,#18054,#18038)
REPRESENTATION_RELATIONSHIP_WITH_TRANSFORMATION(#78)
SHAPE_REPRESENTATION_RELATIONSHIP()
);
#152=(
REPRESENTATION_RELATIONSHIP($,$,#18047,#18046)
REPRESENTATION_RELATIONSHIP_WITH_TRANSFORMATION(#79)
SHAPE_REPRESENTATION_RELATIONSHIP()
);
#153=(
REPRESENTATION_RELATIONSHIP($,$,#18048,#18046)
REPRESENTATION_RELATIONSHIP_WITH_TRANSFORMATION(#80)
SHAPE_REPRESENTATION_RELATIONSHIP()
);
#154=(
REPRESENTATION_RELATIONSHIP($,$,#18049,#18046)
REPRESENTATION_RELATIONSHIP_WITH_TRANSFORMATION(#81)
SHAPE_REPRESENTATION_RELATIONSHIP()
);
#155=(
REPRESENTATION_RELATIONSHIP($,$,#18050,#18046)
REPRESENTATION_RELATIONSHIP_WITH_TRANSFORMATION(#82)
SHAPE_REPRESENTATION_RELATIONSHIP()
);
#156=(
REPRESENTATION_RELATIONSHIP($,$,#18051,#18046)
REPRESENTATION_RELATIONSHIP_WITH_TRANSFORMATION(#83)
SHAPE_REPRESENTATION_RELATIONSHIP()
);
#157=(
REPRESENTATION_RELATIONSHIP($,$,#18052,#18046)
REPRESENTATION_RELATIONSHIP_WITH_TRANSFORMATION(#84)
SHAPE_REPRESENTATION_RELATIONSHIP()
);
#158=(
REPRESENTATION_RELATIONSHIP($,$,#18053,#18046)
REPRESENTATION_RELATIONSHIP_WITH_TRANSFORMATION(#85)
SHAPE_REPRESENTATION_RELATIONSHIP()
);
#159=(
REPRESENTATION_RELATIONSHIP($,$,#18054,#18046)
REPRESENTATION_RELATIONSHIP_WITH_TRANSFORMATION(#86)
SHAPE_REPRESENTATION_RELATIONSHIP()
);
#160=(
REPRESENTATION_RELATIONSHIP($,$,#18007,#18006)
REPRESENTATION_RELATIONSHIP_WITH_TRANSFORMATION(#87)
SHAPE_REPRESENTATION_RELATIONSHIP()
);
#161=(
REPRESENTATION_RELATIONSHIP($,$,#18038,#18006)
REPRESENTATION_RELATIONSHIP_WITH_TRANSFORMATION(#88)
SHAPE_REPRESENTATION_RELATIONSHIP()
);
#162=(
REPRESENTATION_RELATIONSHIP($,$,#18046,#18006)
REPRESENTATION_RELATIONSHIP_WITH_TRANSFORMATION(#89)
SHAPE_REPRESENTATION_RELATIONSHIP()
);
#163=CONTEXT_DEPENDENT_SHAPE_REPRESENTATION(#90,#17908);
#164=CONTEXT_DEPENDENT_SHAPE_REPRESENTATION(#91,#17909);
#165=CONTEXT_DEPENDENT_SHAPE_REPRESENTATION(#92,#17910);
#166=CONTEXT_DEPENDENT_SHAPE_REPRESENTATION(#93,#17911);
#167=CONTEXT_DEPENDENT_SHAPE_REPRESENTATION(#94,#17912);
#168=CONTEXT_DEPENDENT_SHAPE_REPRESENTATION(#95,#17920);
#169=CONTEXT_DEPENDENT_SHAPE_REPRESENTATION(#96,#17921);
#170=CONTEXT_DEPENDENT_SHAPE_REPRESENTATION(#97,#17922);
#171=CONTEXT_DEPENDENT_SHAPE_REPRESENTATION(#98,#17923);
#172=CONTEXT_DEPENDENT_SHAPE_REPRESENTATION(#99,#17924);
#173=CONTEXT_DEPENDENT_SHAPE_REPRESENTATION(#100,#17943);
#174=CONTEXT_DEPENDENT_SHAPE_REPRESENTATION(#101,#17944);
#175=CONTEXT_DEPENDENT_SHAPE_REPRESENTATION(#102,#17945);
#176=CONTEXT_DEPENDENT_SHAPE_REPRESENTATION(#103,#17946);
#177=CONTEXT_DEPENDENT_SHAPE_REPRESENTATION(#104,#17947);
#178=CONTEXT_DEPENDENT_SHAPE_REPRESENTATION(#105,#17948);
#179=CONTEXT_DEPENDENT_SHAPE_REPRESENTATION(#106,#17949);
#180=CONTEXT_DEPENDENT_SHAPE_REPRESENTATION(#107,#17950);
#181=CONTEXT_DEPENDENT_SHAPE_REPRESENTATION(#108,#17951);
#182=CONTEXT_DEPENDENT_SHAPE_REPRESENTATION(#109,#17952);
#183=CONTEXT_DEPENDENT_SHAPE_REPRESENTATION(#110,#17953);
#184=CONTEXT_DEPENDENT_SHAPE_REPRESENTATION(#111,#17954);
#185=CONTEXT_DEPENDENT_SHAPE_REPRESENTATION(#112,#17955);
#186=CONTEXT_DEPENDENT_SHAPE_REPRESENTATION(#113,#17956);
#187=CONTEXT_DEPENDENT_SHAPE_REPRESENTATION(#114,#17957);
#188=CONTEXT_DEPENDENT_SHAPE_REPRESENTATION(#115,#17958);
#189=CONTEXT_DEPENDENT_SHAPE_REPRESENTATION(#116,#17959);
#190=CONTEXT_DEPENDENT_SHAPE_REPRESENTATION(#117,#17960);
#191=CONTEXT_DEPENDENT_SHAPE_REPRESENTATION(#118,#17961);
#192=CONTEXT_DEPENDENT_SHAPE_REPRESENTATION(#119,#17962);
#193=CONTEXT_DEPENDENT_SHAPE_REPRESENTATION(#120,#17963);
#194=CONTEXT_DEPENDENT_SHAPE_REPRESENTATION(#121,#17964);
#195=CONTEXT_DEPENDENT_SHAPE_REPRESENTATION(#122,#17965);
#196=CONTEXT_DEPENDENT_SHAPE_REPRESENTATION(#123,#17966);
#197=CONTEXT_DEPENDENT_SHAPE_REPRESENTATION(#124,#17967);
#198=CONTEXT_DEPENDENT_SHAPE_REPRESENTATION(#125,#17968);
#199=CONTEXT_DEPENDENT_SHAPE_REPRESENTATION(#126,#17969);
#200=CONTEXT_DEPENDENT_SHAPE_REPRESENTATION(#127,#17970);
#201=CONTEXT_DEPENDENT_SHAPE_REPRESENTATION(#128,#17971);
#202=CONTEXT_DEPENDENT_SHAPE_REPRESENTATION(#129,#17972);
#203=CONTEXT_DEPENDENT_SHAPE_REPRESENTATION(#130,#17973);
#204=CONTEXT_DEPENDENT_SHAPE_REPRESENTATION(#131,#17974);
#205=CONTEXT_DEPENDENT_SHAPE_REPRESENTATION(#132,#17975);
#206=CONTEXT_DEPENDENT_SHAPE_REPRESENTATION(#133,#17976);
#207=CONTEXT_DEPENDENT_SHAPE_REPRESENTATION(#134,#17977);
#208=CONTEXT_DEPENDENT_SHAPE_REPRESENTATION(#135,#17978);
#209=CONTEXT_DEPENDENT_SHAPE_REPRESENTATION(#136,#17979);
#210=CONTEXT_DEPENDENT_SHAPE_REPRESENTATION(#137,#17980);
#211=CONTEXT_DEPENDENT_SHAPE_REPRESENTATION(#138,#17981);
#212=CONTEXT_DEPENDENT_SHAPE_REPRESENTATION(#139,#17982);
#213=CONTEXT_DEPENDENT_SHAPE_REPRESENTATION(#140,#17983);
#214=CONTEXT_DEPENDENT_SHAPE_REPRESENTATION(#141,#17984);
#215=CONTEXT_DEPENDENT_SHAPE_REPRESENTATION(#142,#17985);
#216=CONTEXT_DEPENDENT_SHAPE_REPRESENTATION(#143,#17986);
#217=CONTEXT_DEPENDENT_SHAPE_REPRESENTATION(#144,#17987);
#218=CONTEXT_DEPENDENT_SHAPE_REPRESENTATION(#145,#17988);
#219=CONTEXT_DEPENDENT_SHAPE_REPRESENTATION(#146,#17989);
#220=CONTEXT_DEPENDENT_SHAPE_REPRESENTATION(#147,#17990);
#221=CONTEXT_DEPENDENT_SHAPE_REPRESENTATION(#148,#17991);
#222=CONTEXT_DEPENDENT_SHAPE_REPRESENTATION(#149,#17992);
#223=CONTEXT_DEPENDENT_SHAPE_REPRESENTATION(#150,#17993);
#224=CONTEXT_DEPENDENT_SHAPE_REPRESENTATION(#151,#17994);
#225=CONTEXT_DEPENDENT_SHAPE_REPRESENTATION(#152,#17995);
#226=CONTEXT_DEPENDENT_SHAPE_REPRESENTATION(#153,#17996);
#227=CONTEXT_DEPENDENT_SHAPE_REPRESENTATION(#154,#17997);
#228=CONTEXT_DEPENDENT_SHAPE_REPRESENTATION(#155,#17998);
#229=CONTEXT_DEPENDENT_SHAPE_REPRESENTATION(#156,#17999);
#230=CONTEXT_DEPENDENT_SHAPE_REPRESENTATION(#157,#18000);
#231=CONTEXT_DEPENDENT_SHAPE_REPRESENTATION(#158,#18001);
#232=CONTEXT_DEPENDENT_SHAPE_REPRESENTATION(#159,#18002);
#233=CONTEXT_DEPENDENT_SHAPE_REPRESENTATION(#160,#18003);
#234=CONTEXT_DEPENDENT_SHAPE_REPRESENTATION(#161,#18004);
#235=CONTEXT_DEPENDENT_SHAPE_REPRESENTATION(#162,#18005);
#236=NEXT_ASSEMBLY_USAGE_OCCURRENCE('Inner ring:1','Inner ring:1',
'Inner ring:1',#18074,#18075,'Inner ring:1');
#237=NEXT_ASSEMBLY_USAGE_OCCURRENCE('Outer ring:1','Outer ring:1',
'Outer ring:1',#18074,#18076,'Outer ring:1');
#238=NEXT_ASSEMBLY_USAGE_OCCURRENCE('Balls:1','Balls:1','Balls:1',#18074,
#18077,'Balls:1');
#239=NEXT_ASSEMBLY_USAGE_OCCURRENCE('Cage:1','Cage:1','Cage:1',#18074,#18078,
'Cage:1');
#240=NEXT_ASSEMBLY_USAGE_OCCURRENCE('Seals 2RS:1','Seals 2RS:1',
'Seals 2RS:1',#18074,#18079,'Seals 2RS:1');
#241=NEXT_ASSEMBLY_USAGE_OCCURRENCE('Inner ring (1):1',
'Inner ring (1):1','Inner ring (1):1',#18081,#18082,'Inner ring (1):1');
#242=NEXT_ASSEMBLY_USAGE_OCCURRENCE('Outer ring (1):1',
'Outer ring (1):1','Outer ring (1):1',#18081,#18083,'Outer ring (1):1');
#243=NEXT_ASSEMBLY_USAGE_OCCURRENCE('Balls (1):1','Balls (1):1',
'Balls (1):1',#18081,#18084,'Balls (1):1');
#244=NEXT_ASSEMBLY_USAGE_OCCURRENCE('Cage (1):1','Cage (1):1',
'Cage (1):1',#18081,#18085,'Cage (1):1');
#245=NEXT_ASSEMBLY_USAGE_OCCURRENCE('Seals 2RS (1):1','Seals 2RS (1):1',
'Seals 2RS (1):1',#18081,#18086,'Seals 2RS (1):1');
#246=NEXT_ASSEMBLY_USAGE_OCCURRENCE('Base:1','Base:1','Base:1',#18057,#18058,
'Base:1');
#247=NEXT_ASSEMBLY_USAGE_OCCURRENCE('Foot:1','Foot:1','Foot:1',#18057,#18059,
'Foot:1');
#248=NEXT_ASSEMBLY_USAGE_OCCURRENCE('Foot (1):1','Foot (1):1',
'Foot (1):1',#18057,#18060,'Foot (1):1');
#249=NEXT_ASSEMBLY_USAGE_OCCURRENCE('Fixed bearing block:1',
'Fixed bearing block:1','Fixed bearing block:1',#18057,#18061,
'Fixed bearing block:1');
#250=NEXT_ASSEMBLY_USAGE_OCCURRENCE('Input outer spacer:1',
'Input outer spacer:1','Input outer spacer:1',#18057,#18062,
'Input outer spacer:1');
#251=NEXT_ASSEMBLY_USAGE_OCCURRENCE('Input bearing cap:1',
'Input bearing cap:1','Input bearing cap:1',#18057,#18063,
'Input bearing cap:1');
#252=NEXT_ASSEMBLY_USAGE_OCCURRENCE('Input bearing cap (1):1',
'Input bearing cap (1):1','Input bearing cap (1):1',#18057,#18064,
'Input bearing cap (1):1');
#253=NEXT_ASSEMBLY_USAGE_OCCURRENCE('Sliding bearing block:1',
'Sliding bearing block:1','Sliding bearing block:1',#18057,#18065,
'Sliding bearing block:1');
#254=NEXT_ASSEMBLY_USAGE_OCCURRENCE('M4 clamp nut:1','M4 clamp nut:1',
'M4 clamp nut:1',#18057,#18066,'M4 clamp nut:1');
#255=NEXT_ASSEMBLY_USAGE_OCCURRENCE('M4 clamp nut (1):1',
'M4 clamp nut (1):1','M4 clamp nut (1):1',#18057,#18067,
'M4 clamp nut (1):1');
#256=NEXT_ASSEMBLY_USAGE_OCCURRENCE('M4 clamp nut (2):1',
'M4 clamp nut (2):1','M4 clamp nut (2):1',#18057,#18068,
'M4 clamp nut (2):1');
#257=NEXT_ASSEMBLY_USAGE_OCCURRENCE('M4 clamp nut (3):1',
'M4 clamp nut (3):1','M4 clamp nut (3):1',#18057,#18069,
'M4 clamp nut (3):1');
#258=NEXT_ASSEMBLY_USAGE_OCCURRENCE('Output outer spacer:1',
'Output outer spacer:1','Output outer spacer:1',#18057,#18070,
'Output outer spacer:1');
#259=NEXT_ASSEMBLY_USAGE_OCCURRENCE('Output bearing cap:1',
'Output bearing cap:1','Output bearing cap:1',#18057,#18071,
'Output bearing cap:1');
#260=NEXT_ASSEMBLY_USAGE_OCCURRENCE('Output bearing cap (1):1',
'Output bearing cap (1):1','Output bearing cap (1):1',#18057,#18072,
'Output bearing cap (1):1');
#261=NEXT_ASSEMBLY_USAGE_OCCURRENCE('Timing belt backing envelope:1',
'Timing belt backing envelope:1','Timing belt backing envelope:1',#18057,
#18073,'Timing belt backing envelope:1');
#262=NEXT_ASSEMBLY_USAGE_OCCURRENCE('Cap Screw - M4x16:2',
'Cap Screw - M4x16:2','Cap Screw - M4x16:2',#18057,#18104,
'Cap Screw - M4x16:2');
#263=NEXT_ASSEMBLY_USAGE_OCCURRENCE('Cap Screw - M4x16:3',
'Cap Screw - M4x16:3','Cap Screw - M4x16:3',#18057,#18104,
'Cap Screw - M4x16:3');
#264=NEXT_ASSEMBLY_USAGE_OCCURRENCE('Cap Screw - M4x16:4',
'Cap Screw - M4x16:4','Cap Screw - M4x16:4',#18057,#18104,
'Cap Screw - M4x16:4');
#265=NEXT_ASSEMBLY_USAGE_OCCURRENCE('Cap Screw - M4x16:5',
'Cap Screw - M4x16:5','Cap Screw - M4x16:5',#18057,#18104,
'Cap Screw - M4x16:5');
#266=NEXT_ASSEMBLY_USAGE_OCCURRENCE(
'Sealed Ball Bearing - 10 x 30 x 9 mm:2',
'Sealed Ball Bearing - 10 x 30 x 9 mm:2',
'Sealed Ball Bearing - 10 x 30 x 9 mm:2',#18057,#18074,
'Sealed Ball Bearing - 10 x 30 x 9 mm:2');
#267=NEXT_ASSEMBLY_USAGE_OCCURRENCE(
'Sealed Ball Bearing - 10 x 30 x 9 mm:3',
'Sealed Ball Bearing - 10 x 30 x 9 mm:3',
'Sealed Ball Bearing - 10 x 30 x 9 mm:3',#18057,#18074,
'Sealed Ball Bearing - 10 x 30 x 9 mm:3');
#268=NEXT_ASSEMBLY_USAGE_OCCURRENCE('M4x10 Cap Screw:2',
'M4x10 Cap Screw:2','M4x10 Cap Screw:2',#18057,#18087,
'M4x10 Cap Screw:2');
#269=NEXT_ASSEMBLY_USAGE_OCCURRENCE('M4x10 Cap Screw:3',
'M4x10 Cap Screw:3','M4x10 Cap Screw:3',#18057,#18087,
'M4x10 Cap Screw:3');
#270=NEXT_ASSEMBLY_USAGE_OCCURRENCE('M4x10 Cap Screw:4',
'M4x10 Cap Screw:4','M4x10 Cap Screw:4',#18057,#18087,
'M4x10 Cap Screw:4');
#271=NEXT_ASSEMBLY_USAGE_OCCURRENCE('M4x10 Cap Screw:5',
'M4x10 Cap Screw:5','M4x10 Cap Screw:5',#18057,#18087,
'M4x10 Cap Screw:5');
#272=NEXT_ASSEMBLY_USAGE_OCCURRENCE('M4x10 Cap Screw:6',
'M4x10 Cap Screw:6','M4x10 Cap Screw:6',#18057,#18087,
'M4x10 Cap Screw:6');
#273=NEXT_ASSEMBLY_USAGE_OCCURRENCE('M4x10 Cap Screw:7',
'M4x10 Cap Screw:7','M4x10 Cap Screw:7',#18057,#18087,
'M4x10 Cap Screw:7');
#274=NEXT_ASSEMBLY_USAGE_OCCURRENCE('M4x10 Cap Screw:8',
'M4x10 Cap Screw:8','M4x10 Cap Screw:8',#18057,#18087,
'M4x10 Cap Screw:8');
#275=NEXT_ASSEMBLY_USAGE_OCCURRENCE('M4x10 Cap Screw:9',
'M4x10 Cap Screw:9','M4x10 Cap Screw:9',#18057,#18087,
'M4x10 Cap Screw:9');
#276=NEXT_ASSEMBLY_USAGE_OCCURRENCE('M4x30 mounting screw:2',
'M4x30 mounting screw:2','M4x30 mounting screw:2',#18057,#18080,
'M4x30 mounting screw:2');
#277=NEXT_ASSEMBLY_USAGE_OCCURRENCE('M4x30 mounting screw:3',
'M4x30 mounting screw:3','M4x30 mounting screw:3',#18057,#18080,
'M4x30 mounting screw:3');
#278=NEXT_ASSEMBLY_USAGE_OCCURRENCE('M4x30 mounting screw:4',
'M4x30 mounting screw:4','M4x30 mounting screw:4',#18057,#18080,
'M4x30 mounting screw:4');
#279=NEXT_ASSEMBLY_USAGE_OCCURRENCE('M4x30 mounting screw:5',
'M4x30 mounting screw:5','M4x30 mounting screw:5',#18057,#18080,
'M4x30 mounting screw:5');
#280=NEXT_ASSEMBLY_USAGE_OCCURRENCE(
'Sealed Ball Bearing - 12 x 32 x 10 mm:2',
'Sealed Ball Bearing - 12 x 32 x 10 mm:2',
'Sealed Ball Bearing - 12 x 32 x 10 mm:2',#18057,#18081,
'Sealed Ball Bearing - 12 x 32 x 10 mm:2');
#281=NEXT_ASSEMBLY_USAGE_OCCURRENCE(
'Sealed Ball Bearing - 12 x 32 x 10 mm:3',
'Sealed Ball Bearing - 12 x 32 x 10 mm:3',
'Sealed Ball Bearing - 12 x 32 x 10 mm:3',#18057,#18081,
'Sealed Ball Bearing - 12 x 32 x 10 mm:3');
#282=NEXT_ASSEMBLY_USAGE_OCCURRENCE('M4x10 Cap Screw:10',
'M4x10 Cap Screw:10','M4x10 Cap Screw:10',#18057,#18087,
'M4x10 Cap Screw:10');
#283=NEXT_ASSEMBLY_USAGE_OCCURRENCE('M4x10 Cap Screw:11',
'M4x10 Cap Screw:11','M4x10 Cap Screw:11',#18057,#18087,
'M4x10 Cap Screw:11');
#284=NEXT_ASSEMBLY_USAGE_OCCURRENCE('M4x10 Cap Screw:12',
'M4x10 Cap Screw:12','M4x10 Cap Screw:12',#18057,#18087,
'M4x10 Cap Screw:12');
#285=NEXT_ASSEMBLY_USAGE_OCCURRENCE('M4x10 Cap Screw:13',
'M4x10 Cap Screw:13','M4x10 Cap Screw:13',#18057,#18087,
'M4x10 Cap Screw:13');
#286=NEXT_ASSEMBLY_USAGE_OCCURRENCE('M4x10 Cap Screw:14',
'M4x10 Cap Screw:14','M4x10 Cap Screw:14',#18057,#18087,
'M4x10 Cap Screw:14');
#287=NEXT_ASSEMBLY_USAGE_OCCURRENCE('M4x10 Cap Screw:15',
'M4x10 Cap Screw:15','M4x10 Cap Screw:15',#18057,#18087,
'M4x10 Cap Screw:15');
#288=NEXT_ASSEMBLY_USAGE_OCCURRENCE('M4x10 Cap Screw:16',
'M4x10 Cap Screw:16','M4x10 Cap Screw:16',#18057,#18087,
'M4x10 Cap Screw:16');
#289=NEXT_ASSEMBLY_USAGE_OCCURRENCE('M4x10 Cap Screw:17',
'M4x10 Cap Screw:17','M4x10 Cap Screw:17',#18057,#18087,
'M4x10 Cap Screw:17');
#290=NEXT_ASSEMBLY_USAGE_OCCURRENCE('Input shaft:1','Input shaft:1',
'Input shaft:1',#18088,#18089,'Input shaft:1');
#291=NEXT_ASSEMBLY_USAGE_OCCURRENCE('Input inner spacer:1',
'Input inner spacer:1','Input inner spacer:1',#18088,#18090,
'Input inner spacer:1');
#292=NEXT_ASSEMBLY_USAGE_OCCURRENCE('Input inner sleeve:1',
'Input inner sleeve:1','Input inner sleeve:1',#18088,#18091,
'Input inner sleeve:1');
#293=NEXT_ASSEMBLY_USAGE_OCCURRENCE('Input M3 set screw:1',
'Input M3 set screw:1','Input M3 set screw:1',#18088,#18092,
'Input M3 set screw:1');
#294=NEXT_ASSEMBLY_USAGE_OCCURRENCE('Input M3 set screw (1):1',
'Input M3 set screw (1):1','Input M3 set screw (1):1',#18088,#18093,
'Input M3 set screw (1):1');
#295=NEXT_ASSEMBLY_USAGE_OCCURRENCE('Input end keeper:1',
'Input end keeper:1','Input end keeper:1',#18088,#18094,
'Input end keeper:1');
#296=NEXT_ASSEMBLY_USAGE_OCCURRENCE(
'Timing Pulley - 2 mm Pitch, 20 Teeth, 8 mm Bore:2',
'Timing Pulley - 2 mm Pitch, 20 Teeth, 8 mm Bore:2',
'Timing Pulley - 2 mm Pitch, 20 Teeth, 8 mm Bore:2',#18088,#18095,
'Timing Pulley - 2 mm Pitch, 20 Teeth, 8 mm Bore:2');
#297=NEXT_ASSEMBLY_USAGE_OCCURRENCE('Cap Screw - M4x16:6',
'Cap Screw - M4x16:6','Cap Screw - M4x16:6',#18088,#18104,
'Cap Screw - M4x16:6');
#298=NEXT_ASSEMBLY_USAGE_OCCURRENCE('Output shaft:1','Output shaft:1',
'Output shaft:1',#18096,#18097,'Output shaft:1');
#299=NEXT_ASSEMBLY_USAGE_OCCURRENCE('Output inner spacer:1',
'Output inner spacer:1','Output inner spacer:1',#18096,#18098,
'Output inner spacer:1');
#300=NEXT_ASSEMBLY_USAGE_OCCURRENCE('Output inner sleeve:1',
'Output inner sleeve:1','Output inner sleeve:1',#18096,#18099,
'Output inner sleeve:1');
#301=NEXT_ASSEMBLY_USAGE_OCCURRENCE('Output M3 set screw:1',
'Output M3 set screw:1','Output M3 set screw:1',#18096,#18100,
'Output M3 set screw:1');
#302=NEXT_ASSEMBLY_USAGE_OCCURRENCE('Output M3 set screw (1):1',
'Output M3 set screw (1):1','Output M3 set screw (1):1',#18096,#18101,
'Output M3 set screw (1):1');
#303=NEXT_ASSEMBLY_USAGE_OCCURRENCE('Output end keeper:1',
'Output end keeper:1','Output end keeper:1',#18096,#18102,
'Output end keeper:1');
#304=NEXT_ASSEMBLY_USAGE_OCCURRENCE(
'Timing Pulley - 2 mm Pitch, 40 Teeth, 12 mm Bore:2',
'Timing Pulley - 2 mm Pitch, 40 Teeth, 12 mm Bore:2',
'Timing Pulley - 2 mm Pitch, 40 Teeth, 12 mm Bore:2',#18096,#18103,
'Timing Pulley - 2 mm Pitch, 40 Teeth, 12 mm Bore:2');
#305=NEXT_ASSEMBLY_USAGE_OCCURRENCE('Cap Screw - M4x16:7',
'Cap Screw - M4x16:7','Cap Screw - M4x16:7',#18096,#18104,
'Cap Screw - M4x16:7');
#306=NEXT_ASSEMBLY_USAGE_OCCURRENCE('Bearing base and belt envelope:1',
'Bearing base and belt envelope:1','Bearing base and belt envelope:1',#18056,
#18057,'Bearing base and belt envelope:1');
#307=NEXT_ASSEMBLY_USAGE_OCCURRENCE('Input pulley and shaft:1',
'Input pulley and shaft:1','Input pulley and shaft:1',#18056,#18088,
'Input pulley and shaft:1');
#308=NEXT_ASSEMBLY_USAGE_OCCURRENCE('Output pulley and shaft:1',
'Output pulley and shaft:1','Output pulley and shaft:1',#18056,#18096,
'Output pulley and shaft:1');
#309=B_SPLINE_CURVE_WITH_KNOTS('',3,(#14805,#14806,#14807,#14808,#14809,
#14810,#14811,#14812,#14813,#14814,#14815,#14816,#14817,#14818,#14819,#14820,
#14821,#14822,#14823,#14824,#14825,#14826),.UNSPECIFIED.,.F.,.F.,(4,2,2,
2,2,2,2,2,2,2,4),(0.0473477652366656,0.126350602536658,0.189525903804987,
0.252701205073317,0.313298422430275,0.373895639787233,0.434492857144191,
0.495090074501149,0.558265375769478,0.621440677037807,0.7004435143378),
 .UNSPECIFIED.);
#310=B_SPLINE_CURVE_WITH_KNOTS('',3,(#14830,#14831,#14832,#14833,#14834,
#14835,#14836,#14837,#14838,#14839,#14840,#14841,#14842,#14843,#14844,#14845,
#14846,#14847,#14848,#14849,#14850,#14851),.UNSPECIFIED.,.F.,.F.,(4,2,2,
2,2,2,2,2,2,2,4),(0.0464897534940957,0.0852567806515119,0.170513561303024,
0.246687263103517,0.308657850341199,0.370628437578881,0.432599024816563,
0.494569612054245,0.570743313854739,0.656000094506251,0.694767121663666),
 .UNSPECIFIED.);
#311=B_SPLINE_CURVE_WITH_KNOTS('',3,(#14857,#14858,#14859,#14860,#14861,
#14862,#14863,#14864,#14865,#14866,#14867,#14868,#14869,#14870,#14871,#14872,
#14873,#14874,#14875,#14876,#14877,#14878),.UNSPECIFIED.,.F.,.F.,(4,2,2,
2,2,2,2,2,2,2,4),(0.0464897534940957,0.0852567806515118,0.170513561303024,
0.246687263103517,0.308657850341199,0.370628437578881,0.432599024816563,
0.494569612054245,0.570743313854738,0.65600009450625,0.694767121663666),
 .UNSPECIFIED.);
#312=B_SPLINE_CURVE_WITH_KNOTS('',3,(#14882,#14883,#14884,#14885,#14886,
#14887,#14888,#14889,#14890,#14891,#14892,#14893,#14894,#14895,#14896,#14897,
#14898,#14899,#14900,#14901,#14902,#14903),.UNSPECIFIED.,.F.,.F.,(4,2,2,
2,2,2,2,2,2,2,4),(0.0464897534940957,0.0852567806515119,0.170513561303024,
0.246687263103517,0.308657850341199,0.370628437578881,0.432599024816563,
0.494569612054245,0.570743313854739,0.656000094506251,0.694767121663666),
 .UNSPECIFIED.);
#313=B_SPLINE_CURVE_WITH_KNOTS('',3,(#14907,#14908,#14909,#14910,#14911,
#14912,#14913,#14914,#14915,#14916,#14917,#14918),.UNSPECIFIED.,.F.,.F.,
(4,2,2,2,2,4),(0.0464897534940957,0.0852567806515119,0.170513561303024,
0.246687263103517,0.308657850341199,0.370628437578881),.UNSPECIFIED.);
#314=B_SPLINE_CURVE_WITH_KNOTS('',3,(#14923,#14924,#14925,#14926,#14927,
#14928,#14929,#14930,#14931,#14932,#14933,#14934),.UNSPECIFIED.,.F.,.F.,
(4,2,2,2,2,4),(0.370628437578881,0.432599024816563,0.494569612054245,0.570743313854738,
0.65600009450625,0.694767121663666),.UNSPECIFIED.);
#315=B_SPLINE_CURVE_WITH_KNOTS('',3,(#14938,#14939,#14940,#14941,#14942,
#14943,#14944,#14945,#14946,#14947,#14948,#14949,#14950,#14951,#14952,#14953,
#14954,#14955,#14956,#14957,#14958,#14959),.UNSPECIFIED.,.F.,.F.,(4,2,2,
2,2,2,2,2,2,2,4),(0.0464897534940957,0.0852567806515121,0.170513561303024,
0.246687263103518,0.308657850341199,0.370628437578881,0.432599024816563,
0.494569612054245,0.570743313854738,0.65600009450625,0.694767121663666),
 .UNSPECIFIED.);
#316=B_SPLINE_CURVE_WITH_KNOTS('',3,(#14963,#14964,#14965,#14966,#14967,
#14968,#14969,#14970,#14971,#14972,#14973,#14974,#14975,#14976,#14977,#14978,
#14979,#14980,#14981,#14982,#14983,#14984),.UNSPECIFIED.,.F.,.F.,(4,2,2,
2,2,2,2,2,2,2,4),(0.0464897534940957,0.0852567806515119,0.170513561303024,
0.246687263103517,0.308657850341199,0.370628437578881,0.432599024816563,
0.494569612054245,0.570743313854738,0.65600009450625,0.694767121663667),
 .UNSPECIFIED.);
#317=B_SPLINE_CURVE_WITH_KNOTS('',3,(#14988,#14989,#14990,#14991,#14992,
#14993,#14994,#14995,#14996,#14997,#14998,#14999,#15000,#15001,#15002,#15003,
#15004,#15005,#15006,#15007,#15008,#15009),.UNSPECIFIED.,.F.,.F.,(4,2,2,
2,2,2,2,2,2,2,4),(0.0464897534940957,0.0852567806515119,0.170513561303024,
0.246687263103517,0.308657850341199,0.370628437578881,0.432599024816563,
0.494569612054245,0.570743313854738,0.65600009450625,0.694767121663666),
 .UNSPECIFIED.);
#318=B_SPLINE_CURVE_WITH_KNOTS('',3,(#15013,#15014,#15015,#15016,#15017,
#15018,#15019,#15020,#15021,#15022,#15023,#15024,#15025,#15026,#15027,#15028,
#15029,#15030,#15031,#15032,#15033,#15034),.UNSPECIFIED.,.F.,.F.,(4,2,2,
2,2,2,2,2,2,2,4),(0.0464897534940957,0.0852567806515119,0.170513561303024,
0.246687263103517,0.308657850341199,0.370628437578881,0.432599024816563,
0.494569612054245,0.570743313854739,0.656000094506251,0.694767121663667),
 .UNSPECIFIED.);
#319=B_SPLINE_CURVE_WITH_KNOTS('',3,(#15042,#15043,#15044,#15045,#15046,
#15047,#15048,#15049,#15050,#15051,#15052,#15053,#15054,#15055,#15056,#15057,
#15058,#15059,#15060,#15061,#15062,#15063),.UNSPECIFIED.,.F.,.F.,(4,2,2,
2,2,2,2,2,2,2,4),(0.0473477652366656,0.126350602536658,0.189525903804987,
0.252701205073316,0.313298422430274,0.373895639787232,0.434492857144191,
0.495090074501149,0.558265375769478,0.621440677037807,0.7004435143378),
 .UNSPECIFIED.);
#320=B_SPLINE_CURVE_WITH_KNOTS('',3,(#15071,#15072,#15073,#15074,#15075,
#15076,#15077,#15078,#15079,#15080,#15081,#15082,#15083,#15084,#15085,#15086,
#15087,#15088,#15089,#15090,#15091,#15092),.UNSPECIFIED.,.F.,.F.,(4,2,2,
2,2,2,2,2,2,2,4),(0.0473477652366656,0.126350602536658,0.189525903804987,
0.252701205073317,0.313298422430275,0.373895639787233,0.434492857144191,
0.495090074501149,0.558265375769478,0.621440677037807,0.7004435143378),
 .UNSPECIFIED.);
#321=B_SPLINE_CURVE_WITH_KNOTS('',3,(#15101,#15102,#15103,#15104,#15105,
#15106,#15107,#15108,#15109,#15110,#15111,#15112),.UNSPECIFIED.,.F.,.F.,
(4,2,2,2,2,4),(0.0473477652366656,0.126350602536658,0.189525903804987,0.252701205073316,
0.313298422430275,0.373895639787233),.UNSPECIFIED.);
#322=B_SPLINE_CURVE_WITH_KNOTS('',3,(#15114,#15115,#15116,#15117,#15118,
#15119,#15120,#15121,#15122,#15123,#15124,#15125),.UNSPECIFIED.,.F.,.F.,
(4,2,2,2,2,4),(0.373895639787233,0.434492857144191,0.495090074501149,0.558265375769478,
0.621440677037807,0.7004435143378),.UNSPECIFIED.);
#323=B_SPLINE_CURVE_WITH_KNOTS('',3,(#15132,#15133,#15134,#15135,#15136,
#15137,#15138,#15139,#15140,#15141,#15142,#15143,#15144,#15145,#15146,#15147,
#15148,#15149,#15150,#15151,#15152,#15153),.UNSPECIFIED.,.F.,.F.,(4,2,2,
2,2,2,2,2,2,2,4),(0.0473477652366656,0.126350602536658,0.189525903804987,
0.252701205073316,0.313298422430275,0.373895639787233,0.434492857144191,
0.495090074501149,0.558265375769478,0.621440677037807,0.7004435143378),
 .UNSPECIFIED.);
#324=B_SPLINE_CURVE_WITH_KNOTS('',3,(#15161,#15162,#15163,#15164,#15165,
#15166,#15167,#15168,#15169,#15170,#15171,#15172,#15173,#15174,#15175,#15176,
#15177,#15178,#15179,#15180,#15181,#15182),.UNSPECIFIED.,.F.,.F.,(4,2,2,
2,2,2,2,2,2,2,4),(0.0473477652366656,0.126350602536658,0.189525903804987,
0.252701205073317,0.313298422430275,0.373895639787233,0.434492857144191,
0.495090074501149,0.558265375769478,0.621440677037807,0.7004435143378),
 .UNSPECIFIED.);
#325=B_SPLINE_CURVE_WITH_KNOTS('',3,(#15190,#15191,#15192,#15193,#15194,
#15195,#15196,#15197,#15198,#15199,#15200,#15201,#15202,#15203,#15204,#15205,
#15206,#15207,#15208,#15209,#15210,#15211),.UNSPECIFIED.,.F.,.F.,(4,2,2,
2,2,2,2,2,2,2,4),(0.0473477652366656,0.126350602536658,0.189525903804987,
0.252701205073316,0.313298422430275,0.373895639787233,0.434492857144191,
0.495090074501149,0.558265375769478,0.621440677037807,0.7004435143378),
 .UNSPECIFIED.);
#326=B_SPLINE_CURVE_WITH_KNOTS('',3,(#15220,#15221,#15222,#15223,#15224,
#15225,#15226,#15227,#15228,#15229,#15230,#15231,#15232,#15233,#15234,#15235,
#15236,#15237,#15238,#15239,#15240,#15241),.UNSPECIFIED.,.F.,.F.,(4,2,2,
2,2,2,2,2,2,2,4),(0.0473477652366656,0.126350602536658,0.189525903804987,
0.252701205073317,0.313298422430275,0.373895639787233,0.434492857144191,
0.495090074501149,0.558265375769478,0.621440677037807,0.7004435143378),
 .UNSPECIFIED.);
#327=B_SPLINE_CURVE_WITH_KNOTS('',3,(#15464,#15465,#15466,#15467,#15468,
#15469,#15470,#15471,#15472,#15473,#15474,#15475,#15476,#15477,#15478,#15479,
#15480,#15481,#15482,#15483,#15484,#15485),.UNSPECIFIED.,.F.,.F.,(4,2,2,
2,2,2,2,2,2,2,4),(0.0591825211272536,0.157966726598481,0.236950089897721,
0.315933453196962,0.391576304923761,0.46721915665056,0.54286200837736,0.618504860104159,
0.697488223403399,0.77647158670264,0.875255792173867),.UNSPECIFIED.);
#328=B_SPLINE_CURVE_WITH_KNOTS('',3,(#15489,#15490,#15491,#15492,#15493,
#15494,#15495,#15496,#15497,#15498,#15499,#15500,#15501,#15502,#15503,#15504,
#15505,#15506,#15507,#15508,#15509,#15510),.UNSPECIFIED.,.F.,.F.,(4,2,2,
2,2,2,2,2,2,2,4),(0.0581119756758434,0.106553146291161,0.213106292582322,
0.30849933801665,0.386091982889075,0.4636846277615,0.541277272633925,0.61886991750635,
0.714262962940678,0.820816109231839,0.869257279847157),.UNSPECIFIED.);
#329=B_SPLINE_CURVE_WITH_KNOTS('',3,(#15516,#15517,#15518,#15519,#15520,
#15521,#15522,#15523,#15524,#15525,#15526,#15527,#15528,#15529,#15530,#15531,
#15532,#15533,#15534,#15535,#15536,#15537),.UNSPECIFIED.,.F.,.F.,(4,2,2,
2,2,2,2,2,2,2,4),(0.0581119756758434,0.106553146291161,0.213106292582322,
0.30849933801665,0.386091982889075,0.4636846277615,0.541277272633925,0.61886991750635,
0.714262962940679,0.820816109231839,0.869257279847157),.UNSPECIFIED.);
#330=B_SPLINE_CURVE_WITH_KNOTS('',3,(#15541,#15542,#15543,#15544,#15545,
#15546,#15547,#15548,#15549,#15550,#15551,#15552,#15553,#15554,#15555,#15556,
#15557,#15558,#15559,#15560,#15561,#15562),.UNSPECIFIED.,.F.,.F.,(4,2,2,
2,2,2,2,2,2,2,4),(0.0581119756758433,0.106553146291161,0.213106292582322,
0.308499338016649,0.386091982889075,0.4636846277615,0.541277272633925,0.61886991750635,
0.714262962940678,0.820816109231839,0.869257279847157),.UNSPECIFIED.);
#331=B_SPLINE_CURVE_WITH_KNOTS('',3,(#15571,#15572,#15573,#15574,#15575,
#15576,#15577,#15578,#15579,#15580,#15581,#15582,#15583,#15584,#15585,#15586,
#15587,#15588,#15589,#15590,#15591,#15592),.UNSPECIFIED.,.F.,.F.,(4,2,2,
2,2,2,2,2,2,2,4),(0.0581119756758433,0.106553146291161,0.213106292582322,
0.30849933801665,0.386091982889075,0.4636846277615,0.541277272633925,0.61886991750635,
0.714262962940678,0.820816109231839,0.869257279847157),.UNSPECIFIED.);
#332=B_SPLINE_CURVE_WITH_KNOTS('',3,(#15596,#15597,#15598,#15599,#15600,
#15601,#15602,#15603,#15604,#15605,#15606,#15607,#15608,#15609,#15610,#15611,
#15612,#15613,#15614,#15615,#15616,#15617),.UNSPECIFIED.,.F.,.F.,(4,2,2,
2,2,2,2,2,2,2,4),(0.0581119756758434,0.106553146291161,0.213106292582322,
0.30849933801665,0.386091982889075,0.4636846277615,0.541277272633925,0.61886991750635,
0.714262962940678,0.820816109231839,0.869257279847157),.UNSPECIFIED.);
#333=B_SPLINE_CURVE_WITH_KNOTS('',3,(#15621,#15622,#15623,#15624,#15625,
#15626,#15627,#15628,#15629,#15630,#15631,#15632,#15633,#15634,#15635,#15636,
#15637,#15638,#15639,#15640,#15641,#15642),.UNSPECIFIED.,.F.,.F.,(4,2,2,
2,2,2,2,2,2,2,4),(0.0581119756758434,0.106553146291161,0.213106292582322,
0.30849933801665,0.386091982889075,0.4636846277615,0.541277272633925,0.61886991750635,
0.714262962940678,0.820816109231839,0.869257279847157),.UNSPECIFIED.);
#334=B_SPLINE_CURVE_WITH_KNOTS('',3,(#15646,#15647,#15648,#15649,#15650,
#15651,#15652,#15653,#15654,#15655,#15656,#15657,#15658,#15659,#15660,#15661,
#15662,#15663,#15664,#15665,#15666,#15667),.UNSPECIFIED.,.F.,.F.,(4,2,2,
2,2,2,2,2,2,2,4),(0.0581119756758433,0.106553146291161,0.213106292582322,
0.30849933801665,0.386091982889075,0.4636846277615,0.541277272633925,0.61886991750635,
0.714262962940678,0.820816109231839,0.869257279847157),.UNSPECIFIED.);
#335=B_SPLINE_CURVE_WITH_KNOTS('',3,(#15675,#15676,#15677,#15678,#15679,
#15680,#15681,#15682,#15683,#15684,#15685,#15686,#15687,#15688,#15689,#15690,
#15691,#15692,#15693,#15694,#15695,#15696),.UNSPECIFIED.,.F.,.F.,(4,2,2,
2,2,2,2,2,2,2,4),(0.0591825211272536,0.157966726598481,0.236950089897721,
0.315933453196962,0.391576304923761,0.467219156650561,0.54286200837736,
0.618504860104159,0.697488223403399,0.77647158670264,0.875255792173867),
 .UNSPECIFIED.);
#336=B_SPLINE_CURVE_WITH_KNOTS('',3,(#15704,#15705,#15706,#15707,#15708,
#15709,#15710,#15711,#15712,#15713,#15714,#15715,#15716,#15717,#15718,#15719,
#15720,#15721,#15722,#15723,#15724,#15725),.UNSPECIFIED.,.F.,.F.,(4,2,2,
2,2,2,2,2,2,2,4),(0.0591825211272536,0.157966726598481,0.236950089897722,
0.315933453196962,0.391576304923761,0.467219156650561,0.54286200837736,
0.618504860104159,0.697488223403399,0.77647158670264,0.875255792173867),
 .UNSPECIFIED.);
#337=B_SPLINE_CURVE_WITH_KNOTS('',3,(#15735,#15736,#15737,#15738,#15739,
#15740,#15741,#15742,#15743,#15744,#15745,#15746,#15747,#15748,#15749,#15750,
#15751,#15752,#15753,#15754,#15755,#15756),.UNSPECIFIED.,.F.,.F.,(4,2,2,
2,2,2,2,2,2,2,4),(0.0591825211272536,0.157966726598481,0.236950089897721,
0.315933453196962,0.391576304923761,0.46721915665056,0.54286200837736,0.618504860104159,
0.697488223403399,0.77647158670264,0.875255792173867),.UNSPECIFIED.);
#338=B_SPLINE_CURVE_WITH_KNOTS('',3,(#15764,#15765,#15766,#15767,#15768,
#15769,#15770,#15771,#15772,#15773,#15774,#15775,#15776,#15777,#15778,#15779,
#15780,#15781,#15782,#15783,#15784,#15785),.UNSPECIFIED.,.F.,.F.,(4,2,2,
2,2,2,2,2,2,2,4),(0.0591825211272536,0.157966726598481,0.236950089897721,
0.315933453196962,0.391576304923761,0.46721915665056,0.542862008377359,
0.618504860104159,0.697488223403399,0.776471586702639,0.875255792173867),
 .UNSPECIFIED.);
#339=B_SPLINE_CURVE_WITH_KNOTS('',3,(#15793,#15794,#15795,#15796,#15797,
#15798,#15799,#15800,#15801,#15802,#15803,#15804,#15805,#15806,#15807,#15808,
#15809,#15810,#15811,#15812,#15813,#15814),.UNSPECIFIED.,.F.,.F.,(4,2,2,
2,2,2,2,2,2,2,4),(0.0591825211272536,0.157966726598481,0.236950089897721,
0.315933453196962,0.391576304923761,0.46721915665056,0.54286200837736,0.618504860104159,
0.697488223403399,0.77647158670264,0.875255792173867),.UNSPECIFIED.);
#340=B_SPLINE_CURVE_WITH_KNOTS('',3,(#15823,#15824,#15825,#15826,#15827,
#15828,#15829,#15830,#15831,#15832,#15833,#15834,#15835,#15836,#15837,#15838,
#15839,#15840,#15841,#15842,#15843,#15844),.UNSPECIFIED.,.F.,.F.,(4,2,2,
2,2,2,2,2,2,2,4),(0.0591825211272536,0.157966726598481,0.236950089897721,
0.315933453196962,0.391576304923761,0.46721915665056,0.542862008377359,
0.618504860104159,0.697488223403399,0.776471586702639,0.875255792173867),
 .UNSPECIFIED.);
#341=B_SPLINE_CURVE_WITH_KNOTS('',3,(#16064,#16065,#16066,#16067,#16068,
#16069,#16070,#16071,#16072,#16073),.UNSPECIFIED.,.F.,.F.,(4,2,2,2,4),(0.566550474129931,
0.613761886174531,0.66097329821913,0.708186965196186,0.755400632173242),
 .UNSPECIFIED.);
#342=B_SPLINE_CURVE_WITH_KNOTS('',3,(#16075,#16076,#16077,#16078,#16079,
#16080,#16081,#16082,#16083,#16084,#16085,#16086,#16087,#16088,#16089,#16090,
#16091,#16092),.UNSPECIFIED.,.F.,.F.,(4,2,2,2,2,2,2,2,4),(0.18885015804331,
0.23606157008791,0.283272982132509,0.330486649109565,0.377700316086621,
0.424913983063677,0.472127650040732,0.519339062085332,0.566550474129931),
 .UNSPECIFIED.);
#343=B_SPLINE_CURVE_WITH_KNOTS('',3,(#16093,#16094,#16095,#16096,#16097,
#16098,#16099,#16100,#16101,#16102),.UNSPECIFIED.,.F.,.F.,(4,2,2,2,4),(0.755400632173242,
0.802614299150298,0.849827966127353,0.897039378171953,0.944250790216552),
 .UNSPECIFIED.);
#344=B_SPLINE_CURVE_WITH_KNOTS('',3,(#16106,#16107,#16108,#16109,#16110,
#16111,#16112,#16113,#16114,#16115),.UNSPECIFIED.,.F.,.F.,(4,2,2,2,4),(0.189723673274825,
0.237146208024627,0.28456874277443,0.33200804466204,0.37944734654965),
 .UNSPECIFIED.);
#345=B_SPLINE_CURVE_WITH_KNOTS('',3,(#16117,#16118,#16119,#16120,#16121,
#16122,#16123,#16124,#16125,#16126),.UNSPECIFIED.,.F.,.F.,(4,2,2,2,4),(0.,
0.0474393018876097,0.0948786037752193,0.142301138525022,0.189723673274825),
 .UNSPECIFIED.);
#346=B_SPLINE_CURVE_WITH_KNOTS('',3,(#16128,#16129,#16130,#16131,#16132,
#16133,#16134,#16135,#16136,#16137),.UNSPECIFIED.,.F.,.F.,(4,2,2,2,4),(0.569171019824474,
0.616593554574277,0.66401608932408,0.711455391211689,0.758894693099299),
 .UNSPECIFIED.);
#347=B_SPLINE_CURVE_WITH_KNOTS('',3,(#16138,#16139,#16140,#16141,#16142,
#16143,#16144,#16145,#16146,#16147),.UNSPECIFIED.,.F.,.F.,(4,2,2,2,4),(0.37944734654965,
0.426886648437259,0.474325950324869,0.521748485074671,0.569171019824474),
 .UNSPECIFIED.);
#348=B_SPLINE_CURVE_WITH_KNOTS('',3,(#16151,#16152,#16153,#16154,#16155,
#16156,#16157,#16158,#16159,#16160,#16161,#16162,#16163,#16164,#16165,#16166,
#16167,#16168),.UNSPECIFIED.,.F.,.F.,(4,2,2,2,2,2,2,2,4),(0.,0.0474393018876097,
0.0948786037752194,0.142301138525022,0.189723673274825,0.237146208024628,
0.28456874277443,0.33200804466204,0.37944734654965),.UNSPECIFIED.);
#349=B_SPLINE_CURVE_WITH_KNOTS('',3,(#16169,#16170,#16171,#16172,#16173,
#16174,#16175,#16176,#16177,#16178,#16179,#16180,#16181,#16182,#16183,#16184,
#16185,#16186),.UNSPECIFIED.,.F.,.F.,(4,2,2,2,2,2,2,2,4),(0.37944734654965,
0.426886648437259,0.474325950324869,0.521748485074672,0.569171019824474,
0.616593554574277,0.66401608932408,0.711455391211689,0.758894693099299),
 .UNSPECIFIED.);
#350=B_SPLINE_CURVE_WITH_KNOTS('',3,(#16190,#16191,#16192,#16193,#16194,
#16195,#16196,#16197,#16198,#16199),.UNSPECIFIED.,.F.,.F.,(4,2,2,2,4),(0.566550474129931,
0.613761886174531,0.66097329821913,0.708186965196186,0.755400632173242),
 .UNSPECIFIED.);
#351=B_SPLINE_CURVE_WITH_KNOTS('',3,(#16201,#16202,#16203,#16204,#16205,
#16206,#16207,#16208,#16209,#16210,#16211,#16212,#16213,#16214,#16215,#16216,
#16217,#16218),.UNSPECIFIED.,.F.,.F.,(4,2,2,2,2,2,2,2,4),(0.188850158043311,
0.23606157008791,0.283272982132509,0.330486649109565,0.377700316086621,
0.424913983063677,0.472127650040733,0.519339062085332,0.566550474129931),
 .UNSPECIFIED.);
#352=B_SPLINE_CURVE_WITH_KNOTS('',3,(#16219,#16220,#16221,#16222,#16223,
#16224,#16225,#16226,#16227,#16228),.UNSPECIFIED.,.F.,.F.,(4,2,2,2,4),(0.755400632173242,
0.802614299150298,0.849827966127354,0.897039378171953,0.944250790216552),
 .UNSPECIFIED.);
#353=B_SPLINE_CURVE_WITH_KNOTS('',3,(#16238,#16239,#16240,#16241,#16242,
#16243,#16244,#16245,#16246,#16247,#16248,#16249,#16250,#16251,#16252,#16253,
#16254,#16255),.UNSPECIFIED.,.F.,.F.,(4,2,2,2,2,2,2,2,4),(0.18885015804331,
0.23606157008791,0.283272982132509,0.330486649109565,0.377700316086621,
0.424913983063677,0.472127650040732,0.519339062085332,0.566550474129931),
 .UNSPECIFIED.);
#354=B_SPLINE_CURVE_WITH_KNOTS('',3,(#16257,#16258,#16259,#16260,#16261,
#16262,#16263,#16264,#16265,#16266),.UNSPECIFIED.,.F.,.F.,(4,2,2,2,4),(0.566550474129931,
0.613761886174531,0.66097329821913,0.708186965196186,0.755400632173242),
 .UNSPECIFIED.);
#355=B_SPLINE_CURVE_WITH_KNOTS('',3,(#16267,#16268,#16269,#16270,#16271,
#16272,#16273,#16274,#16275,#16276),.UNSPECIFIED.,.F.,.F.,(4,2,2,2,4),(0.755400632173242,
0.802614299150298,0.849827966127353,0.897039378171953,0.944250790216552),
 .UNSPECIFIED.);
#356=B_SPLINE_CURVE_WITH_KNOTS('',3,(#16279,#16280,#16281,#16282,#16283,
#16284,#16285,#16286,#16287,#16288,#16289,#16290,#16291,#16292,#16293,#16294,
#16295,#16296),.UNSPECIFIED.,.F.,.F.,(4,2,2,2,2,2,2,2,4),(0.188850158043311,
0.23606157008791,0.283272982132509,0.330486649109565,0.377700316086621,
0.424913983063677,0.472127650040733,0.519339062085332,0.566550474129932),
 .UNSPECIFIED.);
#357=B_SPLINE_CURVE_WITH_KNOTS('',3,(#16298,#16299,#16300,#16301,#16302,
#16303,#16304,#16305,#16306,#16307),.UNSPECIFIED.,.F.,.F.,(4,2,2,2,4),(0.566550474129932,
0.613761886174531,0.66097329821913,0.708186965196186,0.755400632173242),
 .UNSPECIFIED.);
#358=B_SPLINE_CURVE_WITH_KNOTS('',3,(#16308,#16309,#16310,#16311,#16312,
#16313,#16314,#16315,#16316,#16317),.UNSPECIFIED.,.F.,.F.,(4,2,2,2,4),(0.755400632173242,
0.802614299150298,0.849827966127354,0.897039378171953,0.944250790216552),
 .UNSPECIFIED.);
#359=B_SPLINE_CURVE_WITH_KNOTS('',3,(#16322,#16323,#16324,#16325,#16326,
#16327,#16328,#16329,#16330,#16331,#16332,#16333,#16334,#16335,#16336,#16337,
#16338,#16339),.UNSPECIFIED.,.F.,.F.,(4,2,2,2,2,2,2,2,4),(0.,0.0474393018876097,
0.0948786037752193,0.142301138525022,0.189723673274825,0.237146208024627,
0.28456874277443,0.33200804466204,0.37944734654965),.UNSPECIFIED.);
#360=B_SPLINE_CURVE_WITH_KNOTS('',3,(#16340,#16341,#16342,#16343,#16344,
#16345,#16346,#16347,#16348,#16349,#16350,#16351,#16352,#16353,#16354,#16355,
#16356,#16357),.UNSPECIFIED.,.F.,.F.,(4,2,2,2,2,2,2,2,4),(0.37944734654965,
0.426886648437259,0.474325950324869,0.521748485074672,0.569171019824474,
0.616593554574277,0.66401608932408,0.711455391211689,0.758894693099299),
 .UNSPECIFIED.);
#361=B_SPLINE_CURVE_WITH_KNOTS('',3,(#16361,#16362,#16363,#16364,#16365,
#16366,#16367,#16368,#16369,#16370,#16371,#16372,#16373,#16374,#16375,#16376,
#16377,#16378),.UNSPECIFIED.,.F.,.F.,(4,2,2,2,2,2,2,2,4),(0.,0.0474393018876097,
0.0948786037752194,0.142301138525022,0.189723673274825,0.237146208024627,
0.28456874277443,0.33200804466204,0.37944734654965),.UNSPECIFIED.);
#362=B_SPLINE_CURVE_WITH_KNOTS('',3,(#16379,#16380,#16381,#16382,#16383,
#16384,#16385,#16386,#16387,#16388,#16389,#16390,#16391,#16392,#16393,#16394,
#16395,#16396),.UNSPECIFIED.,.F.,.F.,(4,2,2,2,2,2,2,2,4),(0.37944734654965,
0.426886648437259,0.474325950324869,0.521748485074672,0.569171019824474,
0.616593554574277,0.66401608932408,0.711455391211689,0.758894693099299),
 .UNSPECIFIED.);
#363=B_SPLINE_CURVE_WITH_KNOTS('',3,(#16760,#16761,#16762,#16763,#16764,
#16765,#16766,#16767,#16768,#16769),.UNSPECIFIED.,.F.,.F.,(4,2,2,2,4),(0.565665723963061,
0.61280433739166,0.659942950820258,0.70708195805217,0.754220965284082),
 .UNSPECIFIED.);
#364=B_SPLINE_CURVE_WITH_KNOTS('',3,(#16771,#16772,#16773,#16774,#16775,
#16776,#16777,#16778,#16779,#16780,#16781,#16782,#16783,#16784,#16785,#16786,
#16787,#16788),.UNSPECIFIED.,.F.,.F.,(4,2,2,2,2,2,2,2,4),(0.18855524132102,
0.235693854749619,0.282832468178217,0.329971475410129,0.377110482642041,
0.424249489873953,0.471388497105864,0.518527110534463,0.565665723963061),
 .UNSPECIFIED.);
#365=B_SPLINE_CURVE_WITH_KNOTS('',3,(#16789,#16790,#16791,#16792,#16793,
#16794,#16795,#16796,#16797,#16798),.UNSPECIFIED.,.F.,.F.,(4,2,2,2,4),(0.754220965284082,
0.801359972515993,0.848498979747905,0.895637593176504,0.942776206605102),
 .UNSPECIFIED.);
#366=B_SPLINE_CURVE_WITH_KNOTS('',3,(#16802,#16803,#16804,#16805,#16806,
#16807,#16808,#16809,#16810,#16811),.UNSPECIFIED.,.F.,.F.,(4,2,2,2,4),(0.188940047579712,
0.236173496177583,0.283406944775455,0.330643519967439,0.377880095159423),
 .UNSPECIFIED.);
#367=B_SPLINE_CURVE_WITH_KNOTS('',3,(#16813,#16814,#16815,#16816,#16817,
#16818,#16819,#16820,#16821,#16822),.UNSPECIFIED.,.F.,.F.,(4,2,2,2,4),(0.,
0.0472365751919841,0.0944731503839682,0.14170659898184,0.188940047579712),
 .UNSPECIFIED.);
#368=B_SPLINE_CURVE_WITH_KNOTS('',3,(#16824,#16825,#16826,#16827,#16828,
#16829,#16830,#16831,#16832,#16833),.UNSPECIFIED.,.F.,.F.,(4,2,2,2,4),(0.566820142739135,
0.614053591337007,0.661287039934879,0.708523615126863,0.755760190318847),
 .UNSPECIFIED.);
#369=B_SPLINE_CURVE_WITH_KNOTS('',3,(#16834,#16835,#16836,#16837,#16838,
#16839,#16840,#16841,#16842,#16843),.UNSPECIFIED.,.F.,.F.,(4,2,2,2,4),(0.377880095159423,
0.425116670351408,0.472353245543392,0.519586694141263,0.566820142739135),
 .UNSPECIFIED.);
#370=B_SPLINE_CURVE_WITH_KNOTS('',3,(#16847,#16848,#16849,#16850,#16851,
#16852,#16853,#16854,#16855,#16856,#16857,#16858,#16859,#16860,#16861,#16862,
#16863,#16864),.UNSPECIFIED.,.F.,.F.,(4,2,2,2,2,2,2,2,4),(0.,0.0472365751919841,
0.0944731503839683,0.14170659898184,0.188940047579712,0.236173496177583,
0.283406944775455,0.330643519967439,0.377880095159423),.UNSPECIFIED.);
#371=B_SPLINE_CURVE_WITH_KNOTS('',3,(#16865,#16866,#16867,#16868,#16869,
#16870,#16871,#16872,#16873,#16874,#16875,#16876,#16877,#16878,#16879,#16880,
#16881,#16882),.UNSPECIFIED.,.F.,.F.,(4,2,2,2,2,2,2,2,4),(0.377880095159423,
0.425116670351408,0.472353245543392,0.519586694141263,0.566820142739135,
0.614053591337007,0.661287039934879,0.708523615126863,0.755760190318847),
 .UNSPECIFIED.);
#372=B_SPLINE_CURVE_WITH_KNOTS('',3,(#16886,#16887,#16888,#16889,#16890,
#16891,#16892,#16893,#16894,#16895),.UNSPECIFIED.,.F.,.F.,(4,2,2,2,4),(0.565665723963061,
0.61280433739166,0.659942950820258,0.70708195805217,0.754220965284082),
 .UNSPECIFIED.);
#373=B_SPLINE_CURVE_WITH_KNOTS('',3,(#16897,#16898,#16899,#16900,#16901,
#16902,#16903,#16904,#16905,#16906,#16907,#16908,#16909,#16910,#16911,#16912,
#16913,#16914),.UNSPECIFIED.,.F.,.F.,(4,2,2,2,2,2,2,2,4),(0.18855524132102,
0.235693854749619,0.282832468178217,0.329971475410129,0.377110482642041,
0.424249489873953,0.471388497105864,0.518527110534463,0.565665723963061),
 .UNSPECIFIED.);
#374=B_SPLINE_CURVE_WITH_KNOTS('',3,(#16915,#16916,#16917,#16918,#16919,
#16920,#16921,#16922,#16923,#16924),.UNSPECIFIED.,.F.,.F.,(4,2,2,2,4),(0.754220965284082,
0.801359972515993,0.848498979747905,0.895637593176504,0.942776206605102),
 .UNSPECIFIED.);
#375=B_SPLINE_CURVE_WITH_KNOTS('',3,(#16934,#16935,#16936,#16937,#16938,
#16939,#16940,#16941,#16942,#16943,#16944,#16945,#16946,#16947,#16948,#16949,
#16950,#16951),.UNSPECIFIED.,.F.,.F.,(4,2,2,2,2,2,2,2,4),(0.18855524132102,
0.235693854749619,0.282832468178217,0.329971475410129,0.377110482642041,
0.424249489873953,0.471388497105864,0.518527110534463,0.565665723963061),
 .UNSPECIFIED.);
#376=B_SPLINE_CURVE_WITH_KNOTS('',3,(#16953,#16954,#16955,#16956,#16957,
#16958,#16959,#16960,#16961,#16962),.UNSPECIFIED.,.F.,.F.,(4,2,2,2,4),(0.565665723963061,
0.61280433739166,0.659942950820258,0.70708195805217,0.754220965284082),
 .UNSPECIFIED.);
#377=B_SPLINE_CURVE_WITH_KNOTS('',3,(#16963,#16964,#16965,#16966,#16967,
#16968,#16969,#16970,#16971,#16972),.UNSPECIFIED.,.F.,.F.,(4,2,2,2,4),(0.754220965284082,
0.801359972515993,0.848498979747905,0.895637593176504,0.942776206605102),
 .UNSPECIFIED.);
#378=B_SPLINE_CURVE_WITH_KNOTS('',3,(#16975,#16976,#16977,#16978,#16979,
#16980,#16981,#16982,#16983,#16984,#16985,#16986,#16987,#16988,#16989,#16990,
#16991,#16992),.UNSPECIFIED.,.F.,.F.,(4,2,2,2,2,2,2,2,4),(0.18855524132102,
0.235693854749619,0.282832468178217,0.329971475410129,0.377110482642041,
0.424249489873953,0.471388497105864,0.518527110534463,0.565665723963061),
 .UNSPECIFIED.);
#379=B_SPLINE_CURVE_WITH_KNOTS('',3,(#16994,#16995,#16996,#16997,#16998,
#16999,#17000,#17001,#17002,#17003),.UNSPECIFIED.,.F.,.F.,(4,2,2,2,4),(0.565665723963061,
0.61280433739166,0.659942950820258,0.70708195805217,0.754220965284082),
 .UNSPECIFIED.);
#380=B_SPLINE_CURVE_WITH_KNOTS('',3,(#17004,#17005,#17006,#17007,#17008,
#17009,#17010,#17011,#17012,#17013),.UNSPECIFIED.,.F.,.F.,(4,2,2,2,4),(0.754220965284082,
0.801359972515993,0.848498979747905,0.895637593176504,0.942776206605102),
 .UNSPECIFIED.);
#381=B_SPLINE_CURVE_WITH_KNOTS('',3,(#17018,#17019,#17020,#17021,#17022,
#17023,#17024,#17025,#17026,#17027,#17028,#17029,#17030,#17031,#17032,#17033,
#17034,#17035),.UNSPECIFIED.,.F.,.F.,(4,2,2,2,2,2,2,2,4),(0.,0.0472365751919841,
0.0944731503839683,0.14170659898184,0.188940047579712,0.236173496177583,
0.283406944775455,0.330643519967439,0.377880095159424),.UNSPECIFIED.);
#382=B_SPLINE_CURVE_WITH_KNOTS('',3,(#17036,#17037,#17038,#17039,#17040,
#17041,#17042,#17043,#17044,#17045,#17046,#17047,#17048,#17049,#17050,#17051,
#17052,#17053),.UNSPECIFIED.,.F.,.F.,(4,2,2,2,2,2,2,2,4),(0.377880095159424,
0.425116670351408,0.472353245543392,0.519586694141263,0.566820142739135,
0.614053591337007,0.661287039934879,0.708523615126863,0.755760190318847),
 .UNSPECIFIED.);
#383=B_SPLINE_CURVE_WITH_KNOTS('',3,(#17057,#17058,#17059,#17060,#17061,
#17062,#17063,#17064,#17065,#17066,#17067,#17068,#17069,#17070,#17071,#17072,
#17073,#17074),.UNSPECIFIED.,.F.,.F.,(4,2,2,2,2,2,2,2,4),(0.,0.0472365751919841,
0.0944731503839683,0.14170659898184,0.188940047579712,0.236173496177583,
0.283406944775455,0.330643519967439,0.377880095159423),.UNSPECIFIED.);
#384=B_SPLINE_CURVE_WITH_KNOTS('',3,(#17075,#17076,#17077,#17078,#17079,
#17080,#17081,#17082,#17083,#17084,#17085,#17086,#17087,#17088,#17089,#17090,
#17091,#17092),.UNSPECIFIED.,.F.,.F.,(4,2,2,2,2,2,2,2,4),(0.377880095159423,
0.425116670351408,0.472353245543392,0.519586694141263,0.566820142739135,
0.614053591337007,0.661287039934879,0.708523615126863,0.755760190318847),
 .UNSPECIFIED.);
#385=SPHERICAL_SURFACE('',#9918,0.23815);
#386=SPHERICAL_SURFACE('',#9920,0.23815);
#387=SPHERICAL_SURFACE('',#9922,0.23815);
#388=SPHERICAL_SURFACE('',#9924,0.23815);
#389=SPHERICAL_SURFACE('',#9926,0.23815);
#390=SPHERICAL_SURFACE('',#9928,0.23815);
#391=SPHERICAL_SURFACE('',#9930,0.23815);
#392=SPHERICAL_SURFACE('',#9932,0.23815);
#393=SPHERICAL_SURFACE('',#9935,0.247676);
#394=SPHERICAL_SURFACE('',#9951,0.247676);
#395=SPHERICAL_SURFACE('',#9956,0.247676);
#396=SPHERICAL_SURFACE('',#9961,0.247676);
#397=SPHERICAL_SURFACE('',#9966,0.247676);
#398=SPHERICAL_SURFACE('',#9971,0.247676);
#399=SPHERICAL_SURFACE('',#9976,0.247676);
#400=SPHERICAL_SURFACE('',#9984,0.247676);
#401=SPHERICAL_SURFACE('',#10082,0.29765);
#402=SPHERICAL_SURFACE('',#10084,0.29765);
#403=SPHERICAL_SURFACE('',#10086,0.29765);
#404=SPHERICAL_SURFACE('',#10088,0.29765);
#405=SPHERICAL_SURFACE('',#10090,0.29765);
#406=SPHERICAL_SURFACE('',#10092,0.29765);
#407=SPHERICAL_SURFACE('',#10094,0.29765);
#408=SPHERICAL_SURFACE('',#10097,0.309556);
#409=SPHERICAL_SURFACE('',#10113,0.309556);
#410=SPHERICAL_SURFACE('',#10118,0.309556);
#411=SPHERICAL_SURFACE('',#10124,0.309556);
#412=SPHERICAL_SURFACE('',#10129,0.309556);
#413=SPHERICAL_SURFACE('',#10134,0.309556);
#414=SPHERICAL_SURFACE('',#10142,0.309556);
#415=CONICAL_SURFACE('',#9889,0.53,0.785398163397448);
#416=CONICAL_SURFACE('',#9896,0.53,0.785398163397448);
#417=CONICAL_SURFACE('',#9909,1.47,0.785398163397449);
#418=CONICAL_SURFACE('',#9913,1.47,0.785398163397449);
#419=CONICAL_SURFACE('',#10027,0.325,0.785398163397448);
#420=CONICAL_SURFACE('',#10031,0.335,0.785398163397448);
#421=CONICAL_SURFACE('',#10035,0.21,0.463647609000806);
#422=CONICAL_SURFACE('',#10039,0.18,0.785398163397448);
#423=CONICAL_SURFACE('',#10053,0.63,0.785398163397448);
#424=CONICAL_SURFACE('',#10060,0.63,0.785398163397448);
#425=CONICAL_SURFACE('',#10073,1.57,0.785398163397449);
#426=CONICAL_SURFACE('',#10077,1.57,0.785398163397449);
#427=CONICAL_SURFACE('',#10181,0.325,0.785398163397448);
#428=CONICAL_SURFACE('',#10185,0.335,0.785398163397448);
#429=CONICAL_SURFACE('',#10189,0.21,0.463647609000806);
#430=CONICAL_SURFACE('',#10723,0.325,0.785398163397448);
#431=CONICAL_SURFACE('',#10727,0.335,0.785398163397448);
#432=CONICAL_SURFACE('',#10731,0.21,0.463647609000806);
#433=CONICAL_SURFACE('',#10735,0.18,0.785398163397448);
#434=TOROIDAL_SURFACE('',#9878,1.,0.247676);
#435=TOROIDAL_SURFACE('',#9898,1.,0.247676);
#436=TOROIDAL_SURFACE('',#10042,1.1,0.309556);
#437=TOROIDAL_SURFACE('',#10062,1.1,0.309556);
#438=SHAPE_REPRESENTATION_RELATIONSHIP('SRR','None',#18008,#481);
#439=SHAPE_REPRESENTATION_RELATIONSHIP('SRR','None',#18009,#482);
#440=SHAPE_REPRESENTATION_RELATIONSHIP('SRR','None',#18010,#483);
#441=SHAPE_REPRESENTATION_RELATIONSHIP('SRR','None',#18011,#484);
#442=SHAPE_REPRESENTATION_RELATIONSHIP('SRR','None',#18012,#485);
#443=SHAPE_REPRESENTATION_RELATIONSHIP('SRR','None',#18013,#486);
#444=SHAPE_REPRESENTATION_RELATIONSHIP('SRR','None',#18014,#487);
#445=SHAPE_REPRESENTATION_RELATIONSHIP('SRR','None',#18015,#488);
#446=SHAPE_REPRESENTATION_RELATIONSHIP('SRR','None',#18016,#489);
#447=SHAPE_REPRESENTATION_RELATIONSHIP('SRR','None',#18017,#490);
#448=SHAPE_REPRESENTATION_RELATIONSHIP('SRR','None',#18018,#491);
#449=SHAPE_REPRESENTATION_RELATIONSHIP('SRR','None',#18019,#492);
#450=SHAPE_REPRESENTATION_RELATIONSHIP('SRR','None',#18020,#493);
#451=SHAPE_REPRESENTATION_RELATIONSHIP('SRR','None',#18021,#494);
#452=SHAPE_REPRESENTATION_RELATIONSHIP('SRR','None',#18022,#495);
#453=SHAPE_REPRESENTATION_RELATIONSHIP('SRR','None',#18023,#496);
#454=SHAPE_REPRESENTATION_RELATIONSHIP('SRR','None',#18025,#497);
#455=SHAPE_REPRESENTATION_RELATIONSHIP('SRR','None',#18026,#498);
#456=SHAPE_REPRESENTATION_RELATIONSHIP('SRR','None',#18027,#499);
#457=SHAPE_REPRESENTATION_RELATIONSHIP('SRR','None',#18028,#500);
#458=SHAPE_REPRESENTATION_RELATIONSHIP('SRR','None',#18029,#501);
#459=SHAPE_REPRESENTATION_RELATIONSHIP('SRR','None',#18030,#502);
#460=SHAPE_REPRESENTATION_RELATIONSHIP('SRR','None',#18032,#503);
#461=SHAPE_REPRESENTATION_RELATIONSHIP('SRR','None',#18033,#504);
#462=SHAPE_REPRESENTATION_RELATIONSHIP('SRR','None',#18034,#505);
#463=SHAPE_REPRESENTATION_RELATIONSHIP('SRR','None',#18035,#506);
#464=SHAPE_REPRESENTATION_RELATIONSHIP('SRR','None',#18036,#507);
#465=SHAPE_REPRESENTATION_RELATIONSHIP('SRR','None',#18037,#508);
#466=SHAPE_REPRESENTATION_RELATIONSHIP('SRR','None',#18039,#509);
#467=SHAPE_REPRESENTATION_RELATIONSHIP('SRR','None',#18040,#510);
#468=SHAPE_REPRESENTATION_RELATIONSHIP('SRR','None',#18041,#511);
#469=SHAPE_REPRESENTATION_RELATIONSHIP('SRR','None',#18042,#512);
#470=SHAPE_REPRESENTATION_RELATIONSHIP('SRR','None',#18043,#513);
#471=SHAPE_REPRESENTATION_RELATIONSHIP('SRR','None',#18044,#514);
#472=SHAPE_REPRESENTATION_RELATIONSHIP('SRR','None',#18045,#515);
#473=SHAPE_REPRESENTATION_RELATIONSHIP('SRR','None',#18047,#516);
#474=SHAPE_REPRESENTATION_RELATIONSHIP('SRR','None',#18048,#517);
#475=SHAPE_REPRESENTATION_RELATIONSHIP('SRR','None',#18049,#518);
#476=SHAPE_REPRESENTATION_RELATIONSHIP('SRR','None',#18050,#519);
#477=SHAPE_REPRESENTATION_RELATIONSHIP('SRR','None',#18051,#520);
#478=SHAPE_REPRESENTATION_RELATIONSHIP('SRR','None',#18052,#521);
#479=SHAPE_REPRESENTATION_RELATIONSHIP('SRR','None',#18053,#522);
#480=SHAPE_REPRESENTATION_RELATIONSHIP('SRR','None',#18054,#523);
#481=ADVANCED_BREP_SHAPE_REPRESENTATION('',(#582),#17783);
#482=ADVANCED_BREP_SHAPE_REPRESENTATION('',(#583),#17784);
#483=ADVANCED_BREP_SHAPE_REPRESENTATION('',(#584),#17785);
#484=ADVANCED_BREP_SHAPE_REPRESENTATION('',(#585),#17786);
#485=ADVANCED_BREP_SHAPE_REPRESENTATION('',(#586),#17787);
#486=ADVANCED_BREP_SHAPE_REPRESENTATION('',(#587),#17788);
#487=ADVANCED_BREP_SHAPE_REPRESENTATION('',(#588),#17789);
#488=ADVANCED_BREP_SHAPE_REPRESENTATION('',(#589),#17790);
#489=ADVANCED_BREP_SHAPE_REPRESENTATION('',(#590),#17791);
#490=ADVANCED_BREP_SHAPE_REPRESENTATION('',(#591),#17792);
#491=ADVANCED_BREP_SHAPE_REPRESENTATION('',(#592),#17793);
#492=ADVANCED_BREP_SHAPE_REPRESENTATION('',(#593),#17794);
#493=ADVANCED_BREP_SHAPE_REPRESENTATION('',(#594),#17795);
#494=ADVANCED_BREP_SHAPE_REPRESENTATION('',(#595),#17796);
#495=ADVANCED_BREP_SHAPE_REPRESENTATION('',(#596),#17797);
#496=ADVANCED_BREP_SHAPE_REPRESENTATION('',(#597),#17798);
#497=ADVANCED_BREP_SHAPE_REPRESENTATION('',(#598),#17800);
#498=ADVANCED_BREP_SHAPE_REPRESENTATION('',(#599),#17801);
#499=ADVANCED_BREP_SHAPE_REPRESENTATION('',(#600,#601,#602,#603,#604,#605,
#606,#607),#17802);
#500=ADVANCED_BREP_SHAPE_REPRESENTATION('',(#608),#17803);
#501=ADVANCED_BREP_SHAPE_REPRESENTATION('',(#609,#610),#17804);
#502=ADVANCED_BREP_SHAPE_REPRESENTATION('',(#14),#17805);
#503=ADVANCED_BREP_SHAPE_REPRESENTATION('',(#611),#17807);
#504=ADVANCED_BREP_SHAPE_REPRESENTATION('',(#612),#17808);
#505=ADVANCED_BREP_SHAPE_REPRESENTATION('',(#613,#614,#615,#616,#617,#618,
#619),#17809);
#506=ADVANCED_BREP_SHAPE_REPRESENTATION('',(#620),#17810);
#507=ADVANCED_BREP_SHAPE_REPRESENTATION('',(#621,#622),#17811);
#508=ADVANCED_BREP_SHAPE_REPRESENTATION('',(#15),#17812);
#509=ADVANCED_BREP_SHAPE_REPRESENTATION('',(#623),#17814);
#510=ADVANCED_BREP_SHAPE_REPRESENTATION('',(#624),#17815);
#511=ADVANCED_BREP_SHAPE_REPRESENTATION('',(#625),#17816);
#512=ADVANCED_BREP_SHAPE_REPRESENTATION('',(#626),#17817);
#513=ADVANCED_BREP_SHAPE_REPRESENTATION('',(#627),#17818);
#514=ADVANCED_BREP_SHAPE_REPRESENTATION('',(#628),#17819);
#515=ADVANCED_BREP_SHAPE_REPRESENTATION('',(#629),#17820);
#516=ADVANCED_BREP_SHAPE_REPRESENTATION('',(#630),#17822);
#517=ADVANCED_BREP_SHAPE_REPRESENTATION('',(#631),#17823);
#518=ADVANCED_BREP_SHAPE_REPRESENTATION('',(#632),#17824);
#519=ADVANCED_BREP_SHAPE_REPRESENTATION('',(#633),#17825);
#520=ADVANCED_BREP_SHAPE_REPRESENTATION('',(#634),#17826);
#521=ADVANCED_BREP_SHAPE_REPRESENTATION('',(#635),#17827);
#522=ADVANCED_BREP_SHAPE_REPRESENTATION('',(#636),#17828);
#523=ADVANCED_BREP_SHAPE_REPRESENTATION('',(#16),#17829);
#524=STYLED_ITEM('',(#18296),#582);
#525=STYLED_ITEM('',(#18331),#583);
#526=STYLED_ITEM('',(#18331),#584);
#527=STYLED_ITEM('',(#18317),#585);
#528=STYLED_ITEM('',(#18310),#586);
#529=STYLED_ITEM('',(#18317),#587);
#530=STYLED_ITEM('',(#18317),#588);
#531=STYLED_ITEM('',(#18317),#589);
#532=STYLED_ITEM('',(#18324),#590);
#533=STYLED_ITEM('',(#18324),#591);
#534=STYLED_ITEM('',(#18324),#592);
#535=STYLED_ITEM('',(#18324),#593);
#536=STYLED_ITEM('',(#18331),#594);
#537=STYLED_ITEM('',(#18317),#595);
#538=STYLED_ITEM('',(#18317),#596);
#539=STYLED_ITEM('',(#18324),#597);
#540=STYLED_ITEM('',(#18317),#598);
#541=STYLED_ITEM('',(#18317),#599);
#542=STYLED_ITEM('',(#18317),#600);
#543=STYLED_ITEM('',(#18317),#601);
#544=STYLED_ITEM('',(#18317),#602);
#545=STYLED_ITEM('',(#18317),#603);
#546=STYLED_ITEM('',(#18317),#604);
#547=STYLED_ITEM('',(#18317),#605);
#548=STYLED_ITEM('',(#18317),#606);
#549=STYLED_ITEM('',(#18317),#607);
#550=STYLED_ITEM('',(#18317),#608);
#551=STYLED_ITEM('',(#18317),#609);
#552=STYLED_ITEM('',(#18317),#610);
#553=STYLED_ITEM('',(#18324),#14);
#554=STYLED_ITEM('',(#18317),#611);
#555=STYLED_ITEM('',(#18317),#612);
#556=STYLED_ITEM('',(#18317),#613);
#557=STYLED_ITEM('',(#18317),#614);
#558=STYLED_ITEM('',(#18317),#615);
#559=STYLED_ITEM('',(#18317),#616);
#560=STYLED_ITEM('',(#18317),#617);
#561=STYLED_ITEM('',(#18317),#618);
#562=STYLED_ITEM('',(#18317),#619);
#563=STYLED_ITEM('',(#18317),#620);
#564=STYLED_ITEM('',(#18317),#621);
#565=STYLED_ITEM('',(#18317),#622);
#566=STYLED_ITEM('',(#18324),#15);
#567=STYLED_ITEM('',(#18317),#623);
#568=STYLED_ITEM('',(#18331),#624);
#569=STYLED_ITEM('',(#18303),#625);
#570=STYLED_ITEM('',(#18324),#626);
#571=STYLED_ITEM('',(#18324),#627);
#572=STYLED_ITEM('',(#18310),#628);
#573=STYLED_ITEM('',(#18331),#629);
#574=STYLED_ITEM('',(#18317),#630);
#575=STYLED_ITEM('',(#18310),#631);
#576=STYLED_ITEM('',(#18310),#632);
#577=STYLED_ITEM('',(#18324),#633);
#578=STYLED_ITEM('',(#18324),#634);
#579=STYLED_ITEM('',(#18331),#635);
#580=STYLED_ITEM('',(#18310),#636);
#581=STYLED_ITEM('',(#18324),#16);
#582=MANIFOLD_SOLID_BREP('Body1',#8981);
#583=MANIFOLD_SOLID_BREP('Body1',#8982);
#584=MANIFOLD_SOLID_BREP('Body1',#8983);
#585=MANIFOLD_SOLID_BREP('Body1',#8984);
#586=MANIFOLD_SOLID_BREP('Body1',#8985);
#587=MANIFOLD_SOLID_BREP('Body1',#8986);
#588=MANIFOLD_SOLID_BREP('Body1',#8987);
#589=MANIFOLD_SOLID_BREP('Body1',#8988);
#590=MANIFOLD_SOLID_BREP('Body1',#8989);
#591=MANIFOLD_SOLID_BREP('Body1',#8990);
#592=MANIFOLD_SOLID_BREP('Body1',#8991);
#593=MANIFOLD_SOLID_BREP('Body1',#8992);
#594=MANIFOLD_SOLID_BREP('Body1',#8993);
#595=MANIFOLD_SOLID_BREP('Body1',#8994);
#596=MANIFOLD_SOLID_BREP('Body1',#8995);
#597=MANIFOLD_SOLID_BREP('Body1',#8996);
#598=MANIFOLD_SOLID_BREP('Body1',#8997);
#599=MANIFOLD_SOLID_BREP('Body1',#8998);
#600=MANIFOLD_SOLID_BREP('Body1',#8999);
#601=MANIFOLD_SOLID_BREP('Body2',#9000);
#602=MANIFOLD_SOLID_BREP('Body3',#9001);
#603=MANIFOLD_SOLID_BREP('Body4',#9002);
#604=MANIFOLD_SOLID_BREP('Body5',#9003);
#605=MANIFOLD_SOLID_BREP('Body6',#9004);
#606=MANIFOLD_SOLID_BREP('Body7',#9005);
#607=MANIFOLD_SOLID_BREP('Body8',#9006);
#608=MANIFOLD_SOLID_BREP('Continuous crown cage',#9007);
#609=MANIFOLD_SOLID_BREP('Body1',#9008);
#610=MANIFOLD_SOLID_BREP('Body2',#9009);
#611=MANIFOLD_SOLID_BREP('Body1',#9012);
#612=MANIFOLD_SOLID_BREP('Body1',#9013);
#613=MANIFOLD_SOLID_BREP('Body1',#9014);
#614=MANIFOLD_SOLID_BREP('Body2',#9015);
#615=MANIFOLD_SOLID_BREP('Body3',#9016);
#616=MANIFOLD_SOLID_BREP('Body4',#9017);
#617=MANIFOLD_SOLID_BREP('Body5',#9018);
#618=MANIFOLD_SOLID_BREP('Body6',#9019);
#619=MANIFOLD_SOLID_BREP('Body7',#9020);
#620=MANIFOLD_SOLID_BREP('Continuous crown cage',#9021);
#621=MANIFOLD_SOLID_BREP('Body1',#9022);
#622=MANIFOLD_SOLID_BREP('Body2',#9023);
#623=MANIFOLD_SOLID_BREP('Body1',#9026);
#624=MANIFOLD_SOLID_BREP('Body1',#9027);
#625=MANIFOLD_SOLID_BREP('Body1',#9028);
#626=MANIFOLD_SOLID_BREP('Body1',#9029);
#627=MANIFOLD_SOLID_BREP('Body1',#9030);
#628=MANIFOLD_SOLID_BREP('Body1',#9031);
#629=MANIFOLD_SOLID_BREP('Body1',#9032);
#630=MANIFOLD_SOLID_BREP('Body1',#9033);
#631=MANIFOLD_SOLID_BREP('Body1',#9034);
#632=MANIFOLD_SOLID_BREP('Body1',#9035);
#633=MANIFOLD_SOLID_BREP('Body1',#9036);
#634=MANIFOLD_SOLID_BREP('Body1',#9037);
#635=MANIFOLD_SOLID_BREP('Body1',#9038);
#636=MANIFOLD_SOLID_BREP('Body1',#9039);
#637=FACE_BOUND('',#1486,.T.);
#638=FACE_BOUND('',#1487,.T.);
#639=FACE_BOUND('',#1488,.T.);
#640=FACE_BOUND('',#1489,.T.);
#641=FACE_BOUND('',#1517,.T.);
#642=FACE_BOUND('',#1518,.T.);
#643=FACE_BOUND('',#1519,.T.);
#644=FACE_BOUND('',#1520,.T.);
#645=FACE_BOUND('',#1521,.T.);
#646=FACE_BOUND('',#1522,.T.);
#647=FACE_BOUND('',#1545,.T.);
#648=FACE_BOUND('',#1546,.T.);
#649=FACE_BOUND('',#1548,.T.);
#650=FACE_BOUND('',#1549,.T.);
#651=FACE_BOUND('',#1553,.T.);
#652=FACE_BOUND('',#1554,.T.);
#653=FACE_BOUND('',#1555,.T.);
#654=FACE_BOUND('',#1556,.T.);
#655=FACE_BOUND('',#1557,.T.);
#656=FACE_BOUND('',#1560,.T.);
#657=FACE_BOUND('',#1561,.T.);
#658=FACE_BOUND('',#1562,.T.);
#659=FACE_BOUND('',#1563,.T.);
#660=FACE_BOUND('',#1564,.T.);
#661=FACE_BOUND('',#1568,.T.);
#662=FACE_BOUND('',#1569,.T.);
#663=FACE_BOUND('',#1570,.T.);
#664=FACE_BOUND('',#1571,.T.);
#665=FACE_BOUND('',#1575,.T.);
#666=FACE_BOUND('',#1577,.T.);
#667=FACE_BOUND('',#1583,.T.);
#668=FACE_BOUND('',#1590,.T.);
#669=FACE_BOUND('',#1593,.T.);
#670=FACE_BOUND('',#1599,.T.);
#671=FACE_BOUND('',#1606,.T.);
#672=FACE_BOUND('',#1609,.T.);
#673=FACE_BOUND('',#1620,.T.);
#674=FACE_BOUND('',#1621,.T.);
#675=FACE_BOUND('',#1623,.T.);
#676=FACE_BOUND('',#1624,.T.);
#677=FACE_BOUND('',#1628,.T.);
#678=FACE_BOUND('',#1629,.T.);
#679=FACE_BOUND('',#1630,.T.);
#680=FACE_BOUND('',#1631,.T.);
#681=FACE_BOUND('',#1632,.T.);
#682=FACE_BOUND('',#1635,.T.);
#683=FACE_BOUND('',#1636,.T.);
#684=FACE_BOUND('',#1637,.T.);
#685=FACE_BOUND('',#1638,.T.);
#686=FACE_BOUND('',#1639,.T.);
#687=FACE_BOUND('',#1643,.T.);
#688=FACE_BOUND('',#1644,.T.);
#689=FACE_BOUND('',#1645,.T.);
#690=FACE_BOUND('',#1646,.T.);
#691=FACE_BOUND('',#1650,.T.);
#692=FACE_BOUND('',#1652,.T.);
#693=FACE_BOUND('',#1656,.T.);
#694=FACE_BOUND('',#1658,.T.);
#695=FACE_BOUND('',#1662,.T.);
#696=FACE_BOUND('',#1664,.T.);
#697=FACE_BOUND('',#1668,.T.);
#698=FACE_BOUND('',#1670,.T.);
#699=FACE_BOUND('',#1674,.T.);
#700=FACE_BOUND('',#1676,.T.);
#701=FACE_BOUND('',#1682,.T.);
#702=FACE_BOUND('',#1689,.T.);
#703=FACE_BOUND('',#1692,.T.);
#704=FACE_BOUND('',#1698,.T.);
#705=FACE_BOUND('',#1705,.T.);
#706=FACE_BOUND('',#1708,.T.);
#707=FACE_BOUND('',#1712,.T.);
#708=FACE_BOUND('',#1720,.T.);
#709=FACE_BOUND('',#1726,.T.);
#710=FACE_BOUND('',#1729,.T.);
#711=FACE_BOUND('',#1734,.T.);
#712=FACE_BOUND('',#1739,.T.);
#713=FACE_BOUND('',#1767,.T.);
#714=FACE_BOUND('',#1770,.T.);
#715=FACE_BOUND('',#1773,.T.);
#716=FACE_BOUND('',#1776,.T.);
#717=FACE_BOUND('',#1779,.T.);
#718=FACE_BOUND('',#1790,.T.);
#719=FACE_BOUND('',#1798,.T.);
#720=FACE_BOUND('',#1807,.T.);
#721=FACE_BOUND('',#1810,.T.);
#722=FACE_BOUND('',#1815,.T.);
#723=FACE_BOUND('',#1820,.T.);
#724=FACE_BOUND('',#1845,.T.);
#725=FACE_BOUND('',#1848,.T.);
#726=FACE_BOUND('',#1851,.T.);
#727=FACE_BOUND('',#1854,.T.);
#728=FACE_BOUND('',#1857,.T.);
#729=FACE_BOUND('',#1873,.T.);
#730=FACE_BOUND('',#1879,.T.);
#731=FACE_BOUND('',#1881,.T.);
#732=FACE_BOUND('',#1886,.T.);
#733=FACE_BOUND('',#1890,.T.);
#734=FACE_BOUND('',#1893,.T.);
#735=FACE_BOUND('',#1897,.T.);
#736=FACE_BOUND('',#1899,.T.);
#737=FACE_BOUND('',#1903,.T.);
#738=FACE_BOUND('',#1905,.T.);
#739=FACE_BOUND('',#1915,.T.);
#740=FACE_BOUND('',#1917,.T.);
#741=FACE_BOUND('',#1921,.T.);
#742=FACE_BOUND('',#1922,.T.);
#743=FACE_BOUND('',#1923,.T.);
#744=FACE_BOUND('',#1927,.T.);
#745=FACE_BOUND('',#1928,.T.);
#746=FACE_BOUND('',#1929,.T.);
#747=FACE_BOUND('',#1931,.T.);
#748=FACE_BOUND('',#1933,.T.);
#749=FACE_BOUND('',#1936,.T.);
#750=FACE_BOUND('',#1938,.T.);
#751=FACE_BOUND('',#1941,.T.);
#752=FACE_BOUND('',#1985,.T.);
#753=FACE_BOUND('',#1987,.T.);
#754=FACE_BOUND('',#1991,.T.);
#755=FACE_BOUND('',#1997,.T.);
#756=FACE_BOUND('',#1999,.T.);
#757=FACE_BOUND('',#2003,.T.);
#758=FACE_BOUND('',#2005,.T.);
#759=FACE_BOUND('',#2015,.T.);
#760=FACE_BOUND('',#2017,.T.);
#761=FACE_BOUND('',#2021,.T.);
#762=FACE_BOUND('',#2022,.T.);
#763=FACE_BOUND('',#2023,.T.);
#764=FACE_BOUND('',#2027,.T.);
#765=FACE_BOUND('',#2028,.T.);
#766=FACE_BOUND('',#2029,.T.);
#767=FACE_BOUND('',#2031,.T.);
#768=FACE_BOUND('',#2033,.T.);
#769=FACE_BOUND('',#2036,.T.);
#770=FACE_BOUND('',#2038,.T.);
#771=FACE_BOUND('',#2041,.T.);
#772=FACE_BOUND('',#2127,.T.);
#773=PLANE('',#9525);
#774=PLANE('',#9532);
#775=PLANE('',#9533);
#776=PLANE('',#9538);
#777=PLANE('',#9539);
#778=PLANE('',#9546);
#779=PLANE('',#9547);
#780=PLANE('',#9554);
#781=PLANE('',#9555);
#782=PLANE('',#9559);
#783=PLANE('',#9563);
#784=PLANE('',#9567);
#785=PLANE('',#9571);
#786=PLANE('',#9572);
#787=PLANE('',#9573);
#788=PLANE('',#9574);
#789=PLANE('',#9575);
#790=PLANE('',#9576);
#791=PLANE('',#9578);
#792=PLANE('',#9579);
#793=PLANE('',#9580);
#794=PLANE('',#9581);
#795=PLANE('',#9582);
#796=PLANE('',#9583);
#797=PLANE('',#9585);
#798=PLANE('',#9586);
#799=PLANE('',#9587);
#800=PLANE('',#9588);
#801=PLANE('',#9589);
#802=PLANE('',#9590);
#803=PLANE('',#9619);
#804=PLANE('',#9620);
#805=PLANE('',#9621);
#806=PLANE('',#9622);
#807=PLANE('',#9623);
#808=PLANE('',#9624);
#809=PLANE('',#9625);
#810=PLANE('',#9626);
#811=PLANE('',#9627);
#812=PLANE('',#9628);
#813=PLANE('',#9636);
#814=PLANE('',#9637);
#815=PLANE('',#9651);
#816=PLANE('',#9668);
#817=PLANE('',#9671);
#818=PLANE('',#9685);
#819=PLANE('',#9701);
#820=PLANE('',#9705);
#821=PLANE('',#9734);
#822=PLANE('',#9735);
#823=PLANE('',#9736);
#824=PLANE('',#9737);
#825=PLANE('',#9738);
#826=PLANE('',#9739);
#827=PLANE('',#9740);
#828=PLANE('',#9741);
#829=PLANE('',#9742);
#830=PLANE('',#9743);
#831=PLANE('',#9751);
#832=PLANE('',#9752);
#833=PLANE('',#9760);
#834=PLANE('',#9761);
#835=PLANE('',#9769);
#836=PLANE('',#9770);
#837=PLANE('',#9778);
#838=PLANE('',#9779);
#839=PLANE('',#9787);
#840=PLANE('',#9788);
#841=PLANE('',#9802);
#842=PLANE('',#9819);
#843=PLANE('',#9822);
#844=PLANE('',#9836);
#845=PLANE('',#9852);
#846=PLANE('',#9856);
#847=PLANE('',#9858);
#848=PLANE('',#9859);
#849=PLANE('',#9860);
#850=PLANE('',#9871);
#851=PLANE('',#9872);
#852=PLANE('',#9875);
#853=PLANE('',#9891);
#854=PLANE('',#9894);
#855=PLANE('',#9906);
#856=PLANE('',#9915);
#857=PLANE('',#9948);
#858=PLANE('',#9953);
#859=PLANE('',#9958);
#860=PLANE('',#9963);
#861=PLANE('',#9968);
#862=PLANE('',#9973);
#863=PLANE('',#9982);
#864=PLANE('',#9986);
#865=PLANE('',#9987);
#866=PLANE('',#9989);
#867=PLANE('',#9994);
#868=PLANE('',#9997);
#869=PLANE('',#10002);
#870=PLANE('',#10011);
#871=PLANE('',#10012);
#872=PLANE('',#10013);
#873=PLANE('',#10014);
#874=PLANE('',#10015);
#875=PLANE('',#10016);
#876=PLANE('',#10017);
#877=PLANE('',#10018);
#878=PLANE('',#10019);
#879=PLANE('',#10024);
#880=PLANE('',#10025);
#881=PLANE('',#10033);
#882=PLANE('',#10055);
#883=PLANE('',#10058);
#884=PLANE('',#10070);
#885=PLANE('',#10079);
#886=PLANE('',#10110);
#887=PLANE('',#10115);
#888=PLANE('',#10120);
#889=PLANE('',#10126);
#890=PLANE('',#10131);
#891=PLANE('',#10140);
#892=PLANE('',#10144);
#893=PLANE('',#10145);
#894=PLANE('',#10147);
#895=PLANE('',#10152);
#896=PLANE('',#10155);
#897=PLANE('',#10160);
#898=PLANE('',#10169);
#899=PLANE('',#10170);
#900=PLANE('',#10171);
#901=PLANE('',#10172);
#902=PLANE('',#10173);
#903=PLANE('',#10174);
#904=PLANE('',#10175);
#905=PLANE('',#10176);
#906=PLANE('',#10177);
#907=PLANE('',#10179);
#908=PLANE('',#10187);
#909=PLANE('',#10197);
#910=PLANE('',#10198);
#911=PLANE('',#10201);
#912=PLANE('',#10210);
#913=PLANE('',#10213);
#914=PLANE('',#10214);
#915=PLANE('',#10219);
#916=PLANE('',#10226);
#917=PLANE('',#10227);
#918=PLANE('',#10235);
#919=PLANE('',#10236);
#920=PLANE('',#10241);
#921=PLANE('',#10242);
#922=PLANE('',#10247);
#923=PLANE('',#10248);
#924=PLANE('',#10256);
#925=PLANE('',#10257);
#926=PLANE('',#10269);
#927=PLANE('',#10270);
#928=PLANE('',#10314);
#929=PLANE('',#10315);
#930=PLANE('',#10359);
#931=PLANE('',#10405);
#932=PLANE('',#10406);
#933=PLANE('',#10409);
#934=PLANE('',#10415);
#935=PLANE('',#10418);
#936=PLANE('',#10426);
#937=PLANE('',#10427);
#938=PLANE('',#10435);
#939=PLANE('',#10436);
#940=PLANE('',#10441);
#941=PLANE('',#10442);
#942=PLANE('',#10447);
#943=PLANE('',#10448);
#944=PLANE('',#10456);
#945=PLANE('',#10457);
#946=PLANE('',#10469);
#947=PLANE('',#10470);
#948=PLANE('',#10554);
#949=PLANE('',#10555);
#950=PLANE('',#10639);
#951=PLANE('',#10721);
#952=PLANE('',#10729);
#953=PLANE('',#10737);
#954=PLANE('',#10738);
#955=PLANE('',#10739);
#956=PLANE('',#10740);
#957=PLANE('',#10741);
#958=PLANE('',#10742);
#959=PLANE('',#10743);
#960=PLANE('',#10744);
#961=PLANE('',#10745);
#962=FACE_OUTER_BOUND('',#1483,.T.);
#963=FACE_OUTER_BOUND('',#1484,.T.);
#964=FACE_OUTER_BOUND('',#1485,.T.);
#965=FACE_OUTER_BOUND('',#1490,.T.);
#966=FACE_OUTER_BOUND('',#1491,.T.);
#967=FACE_OUTER_BOUND('',#1492,.T.);
#968=FACE_OUTER_BOUND('',#1493,.T.);
#969=FACE_OUTER_BOUND('',#1494,.T.);
#970=FACE_OUTER_BOUND('',#1495,.T.);
#971=FACE_OUTER_BOUND('',#1496,.T.);
#972=FACE_OUTER_BOUND('',#1497,.T.);
#973=FACE_OUTER_BOUND('',#1498,.T.);
#974=FACE_OUTER_BOUND('',#1499,.T.);
#975=FACE_OUTER_BOUND('',#1500,.T.);
#976=FACE_OUTER_BOUND('',#1501,.T.);
#977=FACE_OUTER_BOUND('',#1502,.T.);
#978=FACE_OUTER_BOUND('',#1503,.T.);
#979=FACE_OUTER_BOUND('',#1504,.T.);
#980=FACE_OUTER_BOUND('',#1505,.T.);
#981=FACE_OUTER_BOUND('',#1506,.T.);
#982=FACE_OUTER_BOUND('',#1507,.T.);
#983=FACE_OUTER_BOUND('',#1508,.T.);
#984=FACE_OUTER_BOUND('',#1509,.T.);
#985=FACE_OUTER_BOUND('',#1510,.T.);
#986=FACE_OUTER_BOUND('',#1511,.T.);
#987=FACE_OUTER_BOUND('',#1512,.T.);
#988=FACE_OUTER_BOUND('',#1513,.T.);
#989=FACE_OUTER_BOUND('',#1514,.T.);
#990=FACE_OUTER_BOUND('',#1515,.T.);
#991=FACE_OUTER_BOUND('',#1516,.T.);
#992=FACE_OUTER_BOUND('',#1523,.T.);
#993=FACE_OUTER_BOUND('',#1524,.T.);
#994=FACE_OUTER_BOUND('',#1525,.T.);
#995=FACE_OUTER_BOUND('',#1526,.T.);
#996=FACE_OUTER_BOUND('',#1527,.T.);
#997=FACE_OUTER_BOUND('',#1528,.T.);
#998=FACE_OUTER_BOUND('',#1529,.T.);
#999=FACE_OUTER_BOUND('',#1530,.T.);
#1000=FACE_OUTER_BOUND('',#1531,.T.);
#1001=FACE_OUTER_BOUND('',#1532,.T.);
#1002=FACE_OUTER_BOUND('',#1533,.T.);
#1003=FACE_OUTER_BOUND('',#1534,.T.);
#1004=FACE_OUTER_BOUND('',#1535,.T.);
#1005=FACE_OUTER_BOUND('',#1536,.T.);
#1006=FACE_OUTER_BOUND('',#1537,.T.);
#1007=FACE_OUTER_BOUND('',#1538,.T.);
#1008=FACE_OUTER_BOUND('',#1539,.T.);
#1009=FACE_OUTER_BOUND('',#1540,.T.);
#1010=FACE_OUTER_BOUND('',#1541,.T.);
#1011=FACE_OUTER_BOUND('',#1542,.T.);
#1012=FACE_OUTER_BOUND('',#1543,.T.);
#1013=FACE_OUTER_BOUND('',#1544,.T.);
#1014=FACE_OUTER_BOUND('',#1547,.T.);
#1015=FACE_OUTER_BOUND('',#1550,.T.);
#1016=FACE_OUTER_BOUND('',#1551,.T.);
#1017=FACE_OUTER_BOUND('',#1552,.T.);
#1018=FACE_OUTER_BOUND('',#1558,.T.);
#1019=FACE_OUTER_BOUND('',#1559,.T.);
#1020=FACE_OUTER_BOUND('',#1565,.T.);
#1021=FACE_OUTER_BOUND('',#1566,.T.);
#1022=FACE_OUTER_BOUND('',#1567,.T.);
#1023=FACE_OUTER_BOUND('',#1572,.T.);
#1024=FACE_OUTER_BOUND('',#1573,.T.);
#1025=FACE_OUTER_BOUND('',#1574,.T.);
#1026=FACE_OUTER_BOUND('',#1576,.T.);
#1027=FACE_OUTER_BOUND('',#1578,.T.);
#1028=FACE_OUTER_BOUND('',#1579,.T.);
#1029=FACE_OUTER_BOUND('',#1580,.T.);
#1030=FACE_OUTER_BOUND('',#1581,.T.);
#1031=FACE_OUTER_BOUND('',#1582,.T.);
#1032=FACE_OUTER_BOUND('',#1584,.T.);
#1033=FACE_OUTER_BOUND('',#1585,.T.);
#1034=FACE_OUTER_BOUND('',#1586,.T.);
#1035=FACE_OUTER_BOUND('',#1587,.T.);
#1036=FACE_OUTER_BOUND('',#1588,.T.);
#1037=FACE_OUTER_BOUND('',#1589,.T.);
#1038=FACE_OUTER_BOUND('',#1591,.T.);
#1039=FACE_OUTER_BOUND('',#1592,.T.);
#1040=FACE_OUTER_BOUND('',#1594,.T.);
#1041=FACE_OUTER_BOUND('',#1595,.T.);
#1042=FACE_OUTER_BOUND('',#1596,.T.);
#1043=FACE_OUTER_BOUND('',#1597,.T.);
#1044=FACE_OUTER_BOUND('',#1598,.T.);
#1045=FACE_OUTER_BOUND('',#1600,.T.);
#1046=FACE_OUTER_BOUND('',#1601,.T.);
#1047=FACE_OUTER_BOUND('',#1602,.T.);
#1048=FACE_OUTER_BOUND('',#1603,.T.);
#1049=FACE_OUTER_BOUND('',#1604,.T.);
#1050=FACE_OUTER_BOUND('',#1605,.T.);
#1051=FACE_OUTER_BOUND('',#1607,.T.);
#1052=FACE_OUTER_BOUND('',#1608,.T.);
#1053=FACE_OUTER_BOUND('',#1610,.T.);
#1054=FACE_OUTER_BOUND('',#1611,.T.);
#1055=FACE_OUTER_BOUND('',#1612,.T.);
#1056=FACE_OUTER_BOUND('',#1613,.T.);
#1057=FACE_OUTER_BOUND('',#1614,.T.);
#1058=FACE_OUTER_BOUND('',#1615,.T.);
#1059=FACE_OUTER_BOUND('',#1616,.T.);
#1060=FACE_OUTER_BOUND('',#1617,.T.);
#1061=FACE_OUTER_BOUND('',#1618,.T.);
#1062=FACE_OUTER_BOUND('',#1619,.T.);
#1063=FACE_OUTER_BOUND('',#1622,.T.);
#1064=FACE_OUTER_BOUND('',#1625,.T.);
#1065=FACE_OUTER_BOUND('',#1626,.T.);
#1066=FACE_OUTER_BOUND('',#1627,.T.);
#1067=FACE_OUTER_BOUND('',#1633,.T.);
#1068=FACE_OUTER_BOUND('',#1634,.T.);
#1069=FACE_OUTER_BOUND('',#1640,.T.);
#1070=FACE_OUTER_BOUND('',#1641,.T.);
#1071=FACE_OUTER_BOUND('',#1642,.T.);
#1072=FACE_OUTER_BOUND('',#1647,.T.);
#1073=FACE_OUTER_BOUND('',#1648,.T.);
#1074=FACE_OUTER_BOUND('',#1649,.T.);
#1075=FACE_OUTER_BOUND('',#1651,.T.);
#1076=FACE_OUTER_BOUND('',#1653,.T.);
#1077=FACE_OUTER_BOUND('',#1654,.T.);
#1078=FACE_OUTER_BOUND('',#1655,.T.);
#1079=FACE_OUTER_BOUND('',#1657,.T.);
#1080=FACE_OUTER_BOUND('',#1659,.T.);
#1081=FACE_OUTER_BOUND('',#1660,.T.);
#1082=FACE_OUTER_BOUND('',#1661,.T.);
#1083=FACE_OUTER_BOUND('',#1663,.T.);
#1084=FACE_OUTER_BOUND('',#1665,.T.);
#1085=FACE_OUTER_BOUND('',#1666,.T.);
#1086=FACE_OUTER_BOUND('',#1667,.T.);
#1087=FACE_OUTER_BOUND('',#1669,.T.);
#1088=FACE_OUTER_BOUND('',#1671,.T.);
#1089=FACE_OUTER_BOUND('',#1672,.T.);
#1090=FACE_OUTER_BOUND('',#1673,.T.);
#1091=FACE_OUTER_BOUND('',#1675,.T.);
#1092=FACE_OUTER_BOUND('',#1677,.T.);
#1093=FACE_OUTER_BOUND('',#1678,.T.);
#1094=FACE_OUTER_BOUND('',#1679,.T.);
#1095=FACE_OUTER_BOUND('',#1680,.T.);
#1096=FACE_OUTER_BOUND('',#1681,.T.);
#1097=FACE_OUTER_BOUND('',#1683,.T.);
#1098=FACE_OUTER_BOUND('',#1684,.T.);
#1099=FACE_OUTER_BOUND('',#1685,.T.);
#1100=FACE_OUTER_BOUND('',#1686,.T.);
#1101=FACE_OUTER_BOUND('',#1687,.T.);
#1102=FACE_OUTER_BOUND('',#1688,.T.);
#1103=FACE_OUTER_BOUND('',#1690,.T.);
#1104=FACE_OUTER_BOUND('',#1691,.T.);
#1105=FACE_OUTER_BOUND('',#1693,.T.);
#1106=FACE_OUTER_BOUND('',#1694,.T.);
#1107=FACE_OUTER_BOUND('',#1695,.T.);
#1108=FACE_OUTER_BOUND('',#1696,.T.);
#1109=FACE_OUTER_BOUND('',#1697,.T.);
#1110=FACE_OUTER_BOUND('',#1699,.T.);
#1111=FACE_OUTER_BOUND('',#1700,.T.);
#1112=FACE_OUTER_BOUND('',#1701,.T.);
#1113=FACE_OUTER_BOUND('',#1702,.T.);
#1114=FACE_OUTER_BOUND('',#1703,.T.);
#1115=FACE_OUTER_BOUND('',#1704,.T.);
#1116=FACE_OUTER_BOUND('',#1706,.T.);
#1117=FACE_OUTER_BOUND('',#1707,.T.);
#1118=FACE_OUTER_BOUND('',#1709,.T.);
#1119=FACE_OUTER_BOUND('',#1710,.T.);
#1120=FACE_OUTER_BOUND('',#1711,.T.);
#1121=FACE_OUTER_BOUND('',#1713,.T.);
#1122=FACE_OUTER_BOUND('',#1714,.T.);
#1123=FACE_OUTER_BOUND('',#1715,.T.);
#1124=FACE_OUTER_BOUND('',#1716,.T.);
#1125=FACE_OUTER_BOUND('',#1717,.T.);
#1126=FACE_OUTER_BOUND('',#1718,.T.);
#1127=FACE_OUTER_BOUND('',#1719,.T.);
#1128=FACE_OUTER_BOUND('',#1721,.T.);
#1129=FACE_OUTER_BOUND('',#1722,.T.);
#1130=FACE_OUTER_BOUND('',#1723,.T.);
#1131=FACE_OUTER_BOUND('',#1724,.T.);
#1132=FACE_OUTER_BOUND('',#1725,.T.);
#1133=FACE_OUTER_BOUND('',#1727,.T.);
#1134=FACE_OUTER_BOUND('',#1728,.T.);
#1135=FACE_OUTER_BOUND('',#1730,.T.);
#1136=FACE_OUTER_BOUND('',#1731,.T.);
#1137=FACE_OUTER_BOUND('',#1732,.T.);
#1138=FACE_OUTER_BOUND('',#1733,.T.);
#1139=FACE_OUTER_BOUND('',#1735,.T.);
#1140=FACE_OUTER_BOUND('',#1736,.T.);
#1141=FACE_OUTER_BOUND('',#1737,.T.);
#1142=FACE_OUTER_BOUND('',#1738,.T.);
#1143=FACE_OUTER_BOUND('',#1740,.T.);
#1144=FACE_OUTER_BOUND('',#1741,.T.);
#1145=FACE_OUTER_BOUND('',#1742,.T.);
#1146=FACE_OUTER_BOUND('',#1743,.T.);
#1147=FACE_OUTER_BOUND('',#1744,.T.);
#1148=FACE_OUTER_BOUND('',#1745,.T.);
#1149=FACE_OUTER_BOUND('',#1746,.T.);
#1150=FACE_OUTER_BOUND('',#1747,.T.);
#1151=FACE_OUTER_BOUND('',#1748,.T.);
#1152=FACE_OUTER_BOUND('',#1749,.T.);
#1153=FACE_OUTER_BOUND('',#1750,.T.);
#1154=FACE_OUTER_BOUND('',#1751,.T.);
#1155=FACE_OUTER_BOUND('',#1752,.T.);
#1156=FACE_OUTER_BOUND('',#1753,.T.);
#1157=FACE_OUTER_BOUND('',#1754,.T.);
#1158=FACE_OUTER_BOUND('',#1755,.T.);
#1159=FACE_OUTER_BOUND('',#1756,.T.);
#1160=FACE_OUTER_BOUND('',#1757,.T.);
#1161=FACE_OUTER_BOUND('',#1758,.T.);
#1162=FACE_OUTER_BOUND('',#1759,.T.);
#1163=FACE_OUTER_BOUND('',#1760,.T.);
#1164=FACE_OUTER_BOUND('',#1761,.T.);
#1165=FACE_OUTER_BOUND('',#1762,.T.);
#1166=FACE_OUTER_BOUND('',#1763,.T.);
#1167=FACE_OUTER_BOUND('',#1764,.T.);
#1168=FACE_OUTER_BOUND('',#1765,.T.);
#1169=FACE_OUTER_BOUND('',#1766,.T.);
#1170=FACE_OUTER_BOUND('',#1768,.T.);
#1171=FACE_OUTER_BOUND('',#1769,.T.);
#1172=FACE_OUTER_BOUND('',#1771,.T.);
#1173=FACE_OUTER_BOUND('',#1772,.T.);
#1174=FACE_OUTER_BOUND('',#1774,.T.);
#1175=FACE_OUTER_BOUND('',#1775,.T.);
#1176=FACE_OUTER_BOUND('',#1777,.T.);
#1177=FACE_OUTER_BOUND('',#1778,.T.);
#1178=FACE_OUTER_BOUND('',#1780,.T.);
#1179=FACE_OUTER_BOUND('',#1781,.T.);
#1180=FACE_OUTER_BOUND('',#1782,.T.);
#1181=FACE_OUTER_BOUND('',#1783,.T.);
#1182=FACE_OUTER_BOUND('',#1784,.T.);
#1183=FACE_OUTER_BOUND('',#1785,.T.);
#1184=FACE_OUTER_BOUND('',#1786,.T.);
#1185=FACE_OUTER_BOUND('',#1787,.T.);
#1186=FACE_OUTER_BOUND('',#1788,.T.);
#1187=FACE_OUTER_BOUND('',#1789,.T.);
#1188=FACE_OUTER_BOUND('',#1791,.T.);
#1189=FACE_OUTER_BOUND('',#1792,.T.);
#1190=FACE_OUTER_BOUND('',#1793,.T.);
#1191=FACE_OUTER_BOUND('',#1794,.T.);
#1192=FACE_OUTER_BOUND('',#1795,.T.);
#1193=FACE_OUTER_BOUND('',#1796,.T.);
#1194=FACE_OUTER_BOUND('',#1797,.T.);
#1195=FACE_OUTER_BOUND('',#1799,.T.);
#1196=FACE_OUTER_BOUND('',#1800,.T.);
#1197=FACE_OUTER_BOUND('',#1801,.T.);
#1198=FACE_OUTER_BOUND('',#1802,.T.);
#1199=FACE_OUTER_BOUND('',#1803,.T.);
#1200=FACE_OUTER_BOUND('',#1804,.T.);
#1201=FACE_OUTER_BOUND('',#1805,.T.);
#1202=FACE_OUTER_BOUND('',#1806,.T.);
#1203=FACE_OUTER_BOUND('',#1808,.T.);
#1204=FACE_OUTER_BOUND('',#1809,.T.);
#1205=FACE_OUTER_BOUND('',#1811,.T.);
#1206=FACE_OUTER_BOUND('',#1812,.T.);
#1207=FACE_OUTER_BOUND('',#1813,.T.);
#1208=FACE_OUTER_BOUND('',#1814,.T.);
#1209=FACE_OUTER_BOUND('',#1816,.T.);
#1210=FACE_OUTER_BOUND('',#1817,.T.);
#1211=FACE_OUTER_BOUND('',#1818,.T.);
#1212=FACE_OUTER_BOUND('',#1819,.T.);
#1213=FACE_OUTER_BOUND('',#1821,.T.);
#1214=FACE_OUTER_BOUND('',#1822,.T.);
#1215=FACE_OUTER_BOUND('',#1823,.T.);
#1216=FACE_OUTER_BOUND('',#1824,.T.);
#1217=FACE_OUTER_BOUND('',#1825,.T.);
#1218=FACE_OUTER_BOUND('',#1826,.T.);
#1219=FACE_OUTER_BOUND('',#1827,.T.);
#1220=FACE_OUTER_BOUND('',#1828,.T.);
#1221=FACE_OUTER_BOUND('',#1829,.T.);
#1222=FACE_OUTER_BOUND('',#1830,.T.);
#1223=FACE_OUTER_BOUND('',#1831,.T.);
#1224=FACE_OUTER_BOUND('',#1832,.T.);
#1225=FACE_OUTER_BOUND('',#1833,.T.);
#1226=FACE_OUTER_BOUND('',#1834,.T.);
#1227=FACE_OUTER_BOUND('',#1835,.T.);
#1228=FACE_OUTER_BOUND('',#1836,.T.);
#1229=FACE_OUTER_BOUND('',#1837,.T.);
#1230=FACE_OUTER_BOUND('',#1838,.T.);
#1231=FACE_OUTER_BOUND('',#1839,.T.);
#1232=FACE_OUTER_BOUND('',#1840,.T.);
#1233=FACE_OUTER_BOUND('',#1841,.T.);
#1234=FACE_OUTER_BOUND('',#1842,.T.);
#1235=FACE_OUTER_BOUND('',#1843,.T.);
#1236=FACE_OUTER_BOUND('',#1844,.T.);
#1237=FACE_OUTER_BOUND('',#1846,.T.);
#1238=FACE_OUTER_BOUND('',#1847,.T.);
#1239=FACE_OUTER_BOUND('',#1849,.T.);
#1240=FACE_OUTER_BOUND('',#1850,.T.);
#1241=FACE_OUTER_BOUND('',#1852,.T.);
#1242=FACE_OUTER_BOUND('',#1853,.T.);
#1243=FACE_OUTER_BOUND('',#1855,.T.);
#1244=FACE_OUTER_BOUND('',#1856,.T.);
#1245=FACE_OUTER_BOUND('',#1858,.T.);
#1246=FACE_OUTER_BOUND('',#1859,.T.);
#1247=FACE_OUTER_BOUND('',#1860,.T.);
#1248=FACE_OUTER_BOUND('',#1861,.T.);
#1249=FACE_OUTER_BOUND('',#1862,.T.);
#1250=FACE_OUTER_BOUND('',#1863,.T.);
#1251=FACE_OUTER_BOUND('',#1864,.T.);
#1252=FACE_OUTER_BOUND('',#1865,.T.);
#1253=FACE_OUTER_BOUND('',#1866,.T.);
#1254=FACE_OUTER_BOUND('',#1867,.T.);
#1255=FACE_OUTER_BOUND('',#1868,.T.);
#1256=FACE_OUTER_BOUND('',#1869,.T.);
#1257=FACE_OUTER_BOUND('',#1870,.T.);
#1258=FACE_OUTER_BOUND('',#1871,.T.);
#1259=FACE_OUTER_BOUND('',#1872,.T.);
#1260=FACE_OUTER_BOUND('',#1874,.T.);
#1261=FACE_OUTER_BOUND('',#1875,.T.);
#1262=FACE_OUTER_BOUND('',#1876,.T.);
#1263=FACE_OUTER_BOUND('',#1877,.T.);
#1264=FACE_OUTER_BOUND('',#1878,.T.);
#1265=FACE_OUTER_BOUND('',#1880,.T.);
#1266=FACE_OUTER_BOUND('',#1882,.T.);
#1267=FACE_OUTER_BOUND('',#1883,.T.);
#1268=FACE_OUTER_BOUND('',#1884,.T.);
#1269=FACE_OUTER_BOUND('',#1885,.T.);
#1270=FACE_OUTER_BOUND('',#1887,.T.);
#1271=FACE_OUTER_BOUND('',#1888,.T.);
#1272=FACE_OUTER_BOUND('',#1889,.T.);
#1273=FACE_OUTER_BOUND('',#1891,.T.);
#1274=FACE_OUTER_BOUND('',#1892,.T.);
#1275=FACE_OUTER_BOUND('',#1894,.T.);
#1276=FACE_OUTER_BOUND('',#1895,.T.);
#1277=FACE_OUTER_BOUND('',#1896,.T.);
#1278=FACE_OUTER_BOUND('',#1898,.T.);
#1279=FACE_OUTER_BOUND('',#1900,.T.);
#1280=FACE_OUTER_BOUND('',#1901,.T.);
#1281=FACE_OUTER_BOUND('',#1902,.T.);
#1282=FACE_OUTER_BOUND('',#1904,.T.);
#1283=FACE_OUTER_BOUND('',#1906,.T.);
#1284=FACE_OUTER_BOUND('',#1907,.T.);
#1285=FACE_OUTER_BOUND('',#1908,.T.);
#1286=FACE_OUTER_BOUND('',#1909,.T.);
#1287=FACE_OUTER_BOUND('',#1910,.T.);
#1288=FACE_OUTER_BOUND('',#1911,.T.);
#1289=FACE_OUTER_BOUND('',#1912,.T.);
#1290=FACE_OUTER_BOUND('',#1913,.T.);
#1291=FACE_OUTER_BOUND('',#1914,.T.);
#1292=FACE_OUTER_BOUND('',#1916,.T.);
#1293=FACE_OUTER_BOUND('',#1918,.T.);
#1294=FACE_OUTER_BOUND('',#1919,.T.);
#1295=FACE_OUTER_BOUND('',#1920,.T.);
#1296=FACE_OUTER_BOUND('',#1924,.T.);
#1297=FACE_OUTER_BOUND('',#1925,.T.);
#1298=FACE_OUTER_BOUND('',#1926,.T.);
#1299=FACE_OUTER_BOUND('',#1930,.T.);
#1300=FACE_OUTER_BOUND('',#1932,.T.);
#1301=FACE_OUTER_BOUND('',#1934,.T.);
#1302=FACE_OUTER_BOUND('',#1935,.T.);
#1303=FACE_OUTER_BOUND('',#1937,.T.);
#1304=FACE_OUTER_BOUND('',#1939,.T.);
#1305=FACE_OUTER_BOUND('',#1940,.T.);
#1306=FACE_OUTER_BOUND('',#1942,.T.);
#1307=FACE_OUTER_BOUND('',#1943,.T.);
#1308=FACE_OUTER_BOUND('',#1944,.T.);
#1309=FACE_OUTER_BOUND('',#1945,.T.);
#1310=FACE_OUTER_BOUND('',#1946,.T.);
#1311=FACE_OUTER_BOUND('',#1947,.T.);
#1312=FACE_OUTER_BOUND('',#1948,.T.);
#1313=FACE_OUTER_BOUND('',#1949,.T.);
#1314=FACE_OUTER_BOUND('',#1950,.T.);
#1315=FACE_OUTER_BOUND('',#1951,.T.);
#1316=FACE_OUTER_BOUND('',#1952,.T.);
#1317=FACE_OUTER_BOUND('',#1953,.T.);
#1318=FACE_OUTER_BOUND('',#1954,.T.);
#1319=FACE_OUTER_BOUND('',#1955,.T.);
#1320=FACE_OUTER_BOUND('',#1956,.T.);
#1321=FACE_OUTER_BOUND('',#1957,.T.);
#1322=FACE_OUTER_BOUND('',#1958,.T.);
#1323=FACE_OUTER_BOUND('',#1959,.T.);
#1324=FACE_OUTER_BOUND('',#1960,.T.);
#1325=FACE_OUTER_BOUND('',#1961,.T.);
#1326=FACE_OUTER_BOUND('',#1962,.T.);
#1327=FACE_OUTER_BOUND('',#1963,.T.);
#1328=FACE_OUTER_BOUND('',#1964,.T.);
#1329=FACE_OUTER_BOUND('',#1965,.T.);
#1330=FACE_OUTER_BOUND('',#1966,.T.);
#1331=FACE_OUTER_BOUND('',#1967,.T.);
#1332=FACE_OUTER_BOUND('',#1968,.T.);
#1333=FACE_OUTER_BOUND('',#1969,.T.);
#1334=FACE_OUTER_BOUND('',#1970,.T.);
#1335=FACE_OUTER_BOUND('',#1971,.T.);
#1336=FACE_OUTER_BOUND('',#1972,.T.);
#1337=FACE_OUTER_BOUND('',#1973,.T.);
#1338=FACE_OUTER_BOUND('',#1974,.T.);
#1339=FACE_OUTER_BOUND('',#1975,.T.);
#1340=FACE_OUTER_BOUND('',#1976,.T.);
#1341=FACE_OUTER_BOUND('',#1977,.T.);
#1342=FACE_OUTER_BOUND('',#1978,.T.);
#1343=FACE_OUTER_BOUND('',#1979,.T.);
#1344=FACE_OUTER_BOUND('',#1980,.T.);
#1345=FACE_OUTER_BOUND('',#1981,.T.);
#1346=FACE_OUTER_BOUND('',#1982,.T.);
#1347=FACE_OUTER_BOUND('',#1983,.T.);
#1348=FACE_OUTER_BOUND('',#1984,.T.);
#1349=FACE_OUTER_BOUND('',#1986,.T.);
#1350=FACE_OUTER_BOUND('',#1988,.T.);
#1351=FACE_OUTER_BOUND('',#1989,.T.);
#1352=FACE_OUTER_BOUND('',#1990,.T.);
#1353=FACE_OUTER_BOUND('',#1992,.T.);
#1354=FACE_OUTER_BOUND('',#1993,.T.);
#1355=FACE_OUTER_BOUND('',#1994,.T.);
#1356=FACE_OUTER_BOUND('',#1995,.T.);
#1357=FACE_OUTER_BOUND('',#1996,.T.);
#1358=FACE_OUTER_BOUND('',#1998,.T.);
#1359=FACE_OUTER_BOUND('',#2000,.T.);
#1360=FACE_OUTER_BOUND('',#2001,.T.);
#1361=FACE_OUTER_BOUND('',#2002,.T.);
#1362=FACE_OUTER_BOUND('',#2004,.T.);
#1363=FACE_OUTER_BOUND('',#2006,.T.);
#1364=FACE_OUTER_BOUND('',#2007,.T.);
#1365=FACE_OUTER_BOUND('',#2008,.T.);
#1366=FACE_OUTER_BOUND('',#2009,.T.);
#1367=FACE_OUTER_BOUND('',#2010,.T.);
#1368=FACE_OUTER_BOUND('',#2011,.T.);
#1369=FACE_OUTER_BOUND('',#2012,.T.);
#1370=FACE_OUTER_BOUND('',#2013,.T.);
#1371=FACE_OUTER_BOUND('',#2014,.T.);
#1372=FACE_OUTER_BOUND('',#2016,.T.);
#1373=FACE_OUTER_BOUND('',#2018,.T.);
#1374=FACE_OUTER_BOUND('',#2019,.T.);
#1375=FACE_OUTER_BOUND('',#2020,.T.);
#1376=FACE_OUTER_BOUND('',#2024,.T.);
#1377=FACE_OUTER_BOUND('',#2025,.T.);
#1378=FACE_OUTER_BOUND('',#2026,.T.);
#1379=FACE_OUTER_BOUND('',#2030,.T.);
#1380=FACE_OUTER_BOUND('',#2032,.T.);
#1381=FACE_OUTER_BOUND('',#2034,.T.);
#1382=FACE_OUTER_BOUND('',#2035,.T.);
#1383=FACE_OUTER_BOUND('',#2037,.T.);
#1384=FACE_OUTER_BOUND('',#2039,.T.);
#1385=FACE_OUTER_BOUND('',#2040,.T.);
#1386=FACE_OUTER_BOUND('',#2042,.T.);
#1387=FACE_OUTER_BOUND('',#2043,.T.);
#1388=FACE_OUTER_BOUND('',#2044,.T.);
#1389=FACE_OUTER_BOUND('',#2045,.T.);
#1390=FACE_OUTER_BOUND('',#2046,.T.);
#1391=FACE_OUTER_BOUND('',#2047,.T.);
#1392=FACE_OUTER_BOUND('',#2048,.T.);
#1393=FACE_OUTER_BOUND('',#2049,.T.);
#1394=FACE_OUTER_BOUND('',#2050,.T.);
#1395=FACE_OUTER_BOUND('',#2051,.T.);
#1396=FACE_OUTER_BOUND('',#2052,.T.);
#1397=FACE_OUTER_BOUND('',#2053,.T.);
#1398=FACE_OUTER_BOUND('',#2054,.T.);
#1399=FACE_OUTER_BOUND('',#2055,.T.);
#1400=FACE_OUTER_BOUND('',#2056,.T.);
#1401=FACE_OUTER_BOUND('',#2057,.T.);
#1402=FACE_OUTER_BOUND('',#2058,.T.);
#1403=FACE_OUTER_BOUND('',#2059,.T.);
#1404=FACE_OUTER_BOUND('',#2060,.T.);
#1405=FACE_OUTER_BOUND('',#2061,.T.);
#1406=FACE_OUTER_BOUND('',#2062,.T.);
#1407=FACE_OUTER_BOUND('',#2063,.T.);
#1408=FACE_OUTER_BOUND('',#2064,.T.);
#1409=FACE_OUTER_BOUND('',#2065,.T.);
#1410=FACE_OUTER_BOUND('',#2066,.T.);
#1411=FACE_OUTER_BOUND('',#2067,.T.);
#1412=FACE_OUTER_BOUND('',#2068,.T.);
#1413=FACE_OUTER_BOUND('',#2069,.T.);
#1414=FACE_OUTER_BOUND('',#2070,.T.);
#1415=FACE_OUTER_BOUND('',#2071,.T.);
#1416=FACE_OUTER_BOUND('',#2072,.T.);
#1417=FACE_OUTER_BOUND('',#2073,.T.);
#1418=FACE_OUTER_BOUND('',#2074,.T.);
#1419=FACE_OUTER_BOUND('',#2075,.T.);
#1420=FACE_OUTER_BOUND('',#2076,.T.);
#1421=FACE_OUTER_BOUND('',#2077,.T.);
#1422=FACE_OUTER_BOUND('',#2078,.T.);
#1423=FACE_OUTER_BOUND('',#2079,.T.);
#1424=FACE_OUTER_BOUND('',#2080,.T.);
#1425=FACE_OUTER_BOUND('',#2081,.T.);
#1426=FACE_OUTER_BOUND('',#2082,.T.);
#1427=FACE_OUTER_BOUND('',#2083,.T.);
#1428=FACE_OUTER_BOUND('',#2084,.T.);
#1429=FACE_OUTER_BOUND('',#2085,.T.);
#1430=FACE_OUTER_BOUND('',#2086,.T.);
#1431=FACE_OUTER_BOUND('',#2087,.T.);
#1432=FACE_OUTER_BOUND('',#2088,.T.);
#1433=FACE_OUTER_BOUND('',#2089,.T.);
#1434=FACE_OUTER_BOUND('',#2090,.T.);
#1435=FACE_OUTER_BOUND('',#2091,.T.);
#1436=FACE_OUTER_BOUND('',#2092,.T.);
#1437=FACE_OUTER_BOUND('',#2093,.T.);
#1438=FACE_OUTER_BOUND('',#2094,.T.);
#1439=FACE_OUTER_BOUND('',#2095,.T.);
#1440=FACE_OUTER_BOUND('',#2096,.T.);
#1441=FACE_OUTER_BOUND('',#2097,.T.);
#1442=FACE_OUTER_BOUND('',#2098,.T.);
#1443=FACE_OUTER_BOUND('',#2099,.T.);
#1444=FACE_OUTER_BOUND('',#2100,.T.);
#1445=FACE_OUTER_BOUND('',#2101,.T.);
#1446=FACE_OUTER_BOUND('',#2102,.T.);
#1447=FACE_OUTER_BOUND('',#2103,.T.);
#1448=FACE_OUTER_BOUND('',#2104,.T.);
#1449=FACE_OUTER_BOUND('',#2105,.T.);
#1450=FACE_OUTER_BOUND('',#2106,.T.);
#1451=FACE_OUTER_BOUND('',#2107,.T.);
#1452=FACE_OUTER_BOUND('',#2108,.T.);
#1453=FACE_OUTER_BOUND('',#2109,.T.);
#1454=FACE_OUTER_BOUND('',#2110,.T.);
#1455=FACE_OUTER_BOUND('',#2111,.T.);
#1456=FACE_OUTER_BOUND('',#2112,.T.);
#1457=FACE_OUTER_BOUND('',#2113,.T.);
#1458=FACE_OUTER_BOUND('',#2114,.T.);
#1459=FACE_OUTER_BOUND('',#2115,.T.);
#1460=FACE_OUTER_BOUND('',#2116,.T.);
#1461=FACE_OUTER_BOUND('',#2117,.T.);
#1462=FACE_OUTER_BOUND('',#2118,.T.);
#1463=FACE_OUTER_BOUND('',#2119,.T.);
#1464=FACE_OUTER_BOUND('',#2120,.T.);
#1465=FACE_OUTER_BOUND('',#2121,.T.);
#1466=FACE_OUTER_BOUND('',#2122,.T.);
#1467=FACE_OUTER_BOUND('',#2123,.T.);
#1468=FACE_OUTER_BOUND('',#2124,.T.);
#1469=FACE_OUTER_BOUND('',#2125,.T.);
#1470=FACE_OUTER_BOUND('',#2126,.T.);
#1471=FACE_OUTER_BOUND('',#2128,.T.);
#1472=FACE_OUTER_BOUND('',#2129,.T.);
#1473=FACE_OUTER_BOUND('',#2130,.T.);
#1474=FACE_OUTER_BOUND('',#2131,.T.);
#1475=FACE_OUTER_BOUND('',#2132,.T.);
#1476=FACE_OUTER_BOUND('',#2133,.T.);
#1477=FACE_OUTER_BOUND('',#2134,.T.);
#1478=FACE_OUTER_BOUND('',#2135,.T.);
#1479=FACE_OUTER_BOUND('',#2136,.T.);
#1480=FACE_OUTER_BOUND('',#2137,.T.);
#1481=FACE_OUTER_BOUND('',#2138,.T.);
#1482=FACE_OUTER_BOUND('',#2139,.T.);
#1483=EDGE_LOOP('',(#5773,#5774,#5775,#5776));
#1484=EDGE_LOOP('',(#5777,#5778,#5779,#5780));
#1485=EDGE_LOOP('',(#5781,#5782,#5783,#5784));
#1486=EDGE_LOOP('',(#5785,#5786,#5787,#5788));
#1487=EDGE_LOOP('',(#5789,#5790,#5791,#5792));
#1488=EDGE_LOOP('',(#5793,#5794,#5795,#5796));
#1489=EDGE_LOOP('',(#5797,#5798,#5799,#5800));
#1490=EDGE_LOOP('',(#5801,#5802,#5803,#5804));
#1491=EDGE_LOOP('',(#5805,#5806,#5807,#5808));
#1492=EDGE_LOOP('',(#5809,#5810,#5811,#5812));
#1493=EDGE_LOOP('',(#5813,#5814,#5815,#5816));
#1494=EDGE_LOOP('',(#5817,#5818,#5819,#5820));
#1495=EDGE_LOOP('',(#5821,#5822,#5823,#5824));
#1496=EDGE_LOOP('',(#5825,#5826,#5827,#5828,#5829,#5830,#5831,#5832));
#1497=EDGE_LOOP('',(#5833,#5834,#5835,#5836));
#1498=EDGE_LOOP('',(#5837,#5838,#5839,#5840));
#1499=EDGE_LOOP('',(#5841,#5842,#5843,#5844));
#1500=EDGE_LOOP('',(#5845,#5846,#5847,#5848,#5849,#5850,#5851,#5852));
#1501=EDGE_LOOP('',(#5853,#5854,#5855,#5856));
#1502=EDGE_LOOP('',(#5857,#5858,#5859,#5860));
#1503=EDGE_LOOP('',(#5861,#5862,#5863,#5864));
#1504=EDGE_LOOP('',(#5865,#5866,#5867,#5868));
#1505=EDGE_LOOP('',(#5869,#5870));
#1506=EDGE_LOOP('',(#5871,#5872,#5873,#5874));
#1507=EDGE_LOOP('',(#5875));
#1508=EDGE_LOOP('',(#5876,#5877,#5878,#5879));
#1509=EDGE_LOOP('',(#5880));
#1510=EDGE_LOOP('',(#5881,#5882,#5883,#5884));
#1511=EDGE_LOOP('',(#5885,#5886));
#1512=EDGE_LOOP('',(#5887,#5888,#5889,#5890));
#1513=EDGE_LOOP('',(#5891,#5892,#5893,#5894));
#1514=EDGE_LOOP('',(#5895,#5896,#5897,#5898));
#1515=EDGE_LOOP('',(#5899,#5900,#5901,#5902));
#1516=EDGE_LOOP('',(#5903,#5904,#5905,#5906));
#1517=EDGE_LOOP('',(#5907,#5908,#5909,#5910));
#1518=EDGE_LOOP('',(#5911,#5912,#5913,#5914));
#1519=EDGE_LOOP('',(#5915,#5916,#5917,#5918,#5919,#5920));
#1520=EDGE_LOOP('',(#5921,#5922,#5923,#5924,#5925,#5926));
#1521=EDGE_LOOP('',(#5927));
#1522=EDGE_LOOP('',(#5928));
#1523=EDGE_LOOP('',(#5929,#5930,#5931,#5932));
#1524=EDGE_LOOP('',(#5933,#5934,#5935,#5936));
#1525=EDGE_LOOP('',(#5937,#5938,#5939,#5940));
#1526=EDGE_LOOP('',(#5941,#5942,#5943,#5944));
#1527=EDGE_LOOP('',(#5945,#5946,#5947,#5948));
#1528=EDGE_LOOP('',(#5949,#5950,#5951,#5952));
#1529=EDGE_LOOP('',(#5953,#5954,#5955,#5956));
#1530=EDGE_LOOP('',(#5957,#5958,#5959,#5960));
#1531=EDGE_LOOP('',(#5961,#5962,#5963,#5964));
#1532=EDGE_LOOP('',(#5965,#5966,#5967,#5968));
#1533=EDGE_LOOP('',(#5969,#5970,#5971,#5972));
#1534=EDGE_LOOP('',(#5973,#5974,#5975,#5976));
#1535=EDGE_LOOP('',(#5977,#5978,#5979,#5980));
#1536=EDGE_LOOP('',(#5981,#5982,#5983,#5984));
#1537=EDGE_LOOP('',(#5985,#5986,#5987,#5988));
#1538=EDGE_LOOP('',(#5989,#5990,#5991,#5992));
#1539=EDGE_LOOP('',(#5993,#5994,#5995,#5996));
#1540=EDGE_LOOP('',(#5997,#5998,#5999,#6000));
#1541=EDGE_LOOP('',(#6001,#6002,#6003,#6004));
#1542=EDGE_LOOP('',(#6005,#6006,#6007,#6008));
#1543=EDGE_LOOP('',(#6009,#6010,#6011,#6012));
#1544=EDGE_LOOP('',(#6013,#6014,#6015,#6016));
#1545=EDGE_LOOP('',(#6017));
#1546=EDGE_LOOP('',(#6018));
#1547=EDGE_LOOP('',(#6019,#6020,#6021,#6022));
#1548=EDGE_LOOP('',(#6023));
#1549=EDGE_LOOP('',(#6024));
#1550=EDGE_LOOP('',(#6025,#6026,#6027,#6028));
#1551=EDGE_LOOP('',(#6029,#6030,#6031,#6032));
#1552=EDGE_LOOP('',(#6033,#6034,#6035,#6036,#6037,#6038,#6039,#6040));
#1553=EDGE_LOOP('',(#6041));
#1554=EDGE_LOOP('',(#6042));
#1555=EDGE_LOOP('',(#6043));
#1556=EDGE_LOOP('',(#6044));
#1557=EDGE_LOOP('',(#6045));
#1558=EDGE_LOOP('',(#6046,#6047,#6048,#6049));
#1559=EDGE_LOOP('',(#6050,#6051,#6052,#6053,#6054,#6055,#6056,#6057));
#1560=EDGE_LOOP('',(#6058));
#1561=EDGE_LOOP('',(#6059));
#1562=EDGE_LOOP('',(#6060));
#1563=EDGE_LOOP('',(#6061));
#1564=EDGE_LOOP('',(#6062));
#1565=EDGE_LOOP('',(#6063,#6064,#6065,#6066));
#1566=EDGE_LOOP('',(#6067,#6068,#6069,#6070));
#1567=EDGE_LOOP('',(#6071,#6072,#6073,#6074));
#1568=EDGE_LOOP('',(#6075));
#1569=EDGE_LOOP('',(#6076));
#1570=EDGE_LOOP('',(#6077));
#1571=EDGE_LOOP('',(#6078));
#1572=EDGE_LOOP('',(#6079,#6080,#6081,#6082));
#1573=EDGE_LOOP('',(#6083,#6084,#6085,#6086));
#1574=EDGE_LOOP('',(#6087));
#1575=EDGE_LOOP('',(#6088));
#1576=EDGE_LOOP('',(#6089));
#1577=EDGE_LOOP('',(#6090));
#1578=EDGE_LOOP('',(#6091,#6092,#6093,#6094));
#1579=EDGE_LOOP('',(#6095,#6096,#6097,#6098));
#1580=EDGE_LOOP('',(#6099,#6100,#6101,#6102));
#1581=EDGE_LOOP('',(#6103,#6104,#6105,#6106));
#1582=EDGE_LOOP('',(#6107,#6108,#6109,#6110,#6111,#6112,#6113,#6114));
#1583=EDGE_LOOP('',(#6115));
#1584=EDGE_LOOP('',(#6116,#6117,#6118,#6119));
#1585=EDGE_LOOP('',(#6120,#6121,#6122,#6123));
#1586=EDGE_LOOP('',(#6124,#6125,#6126,#6127));
#1587=EDGE_LOOP('',(#6128,#6129,#6130,#6131));
#1588=EDGE_LOOP('',(#6132,#6133,#6134,#6135));
#1589=EDGE_LOOP('',(#6136));
#1590=EDGE_LOOP('',(#6137));
#1591=EDGE_LOOP('',(#6138,#6139,#6140,#6141));
#1592=EDGE_LOOP('',(#6142,#6143,#6144,#6145,#6146,#6147,#6148,#6149));
#1593=EDGE_LOOP('',(#6150));
#1594=EDGE_LOOP('',(#6151,#6152,#6153,#6154));
#1595=EDGE_LOOP('',(#6155,#6156,#6157,#6158));
#1596=EDGE_LOOP('',(#6159,#6160,#6161,#6162));
#1597=EDGE_LOOP('',(#6163,#6164,#6165,#6166));
#1598=EDGE_LOOP('',(#6167,#6168,#6169,#6170,#6171,#6172,#6173,#6174));
#1599=EDGE_LOOP('',(#6175));
#1600=EDGE_LOOP('',(#6176,#6177,#6178,#6179));
#1601=EDGE_LOOP('',(#6180,#6181,#6182,#6183));
#1602=EDGE_LOOP('',(#6184,#6185,#6186,#6187));
#1603=EDGE_LOOP('',(#6188,#6189,#6190,#6191));
#1604=EDGE_LOOP('',(#6192,#6193,#6194,#6195));
#1605=EDGE_LOOP('',(#6196));
#1606=EDGE_LOOP('',(#6197));
#1607=EDGE_LOOP('',(#6198,#6199,#6200,#6201));
#1608=EDGE_LOOP('',(#6202,#6203,#6204,#6205,#6206,#6207,#6208,#6209));
#1609=EDGE_LOOP('',(#6210));
#1610=EDGE_LOOP('',(#6211,#6212,#6213,#6214));
#1611=EDGE_LOOP('',(#6215,#6216,#6217,#6218));
#1612=EDGE_LOOP('',(#6219,#6220,#6221,#6222));
#1613=EDGE_LOOP('',(#6223,#6224,#6225,#6226));
#1614=EDGE_LOOP('',(#6227,#6228,#6229,#6230));
#1615=EDGE_LOOP('',(#6231,#6232,#6233,#6234));
#1616=EDGE_LOOP('',(#6235,#6236,#6237,#6238));
#1617=EDGE_LOOP('',(#6239,#6240,#6241,#6242));
#1618=EDGE_LOOP('',(#6243,#6244,#6245,#6246));
#1619=EDGE_LOOP('',(#6247,#6248,#6249,#6250));
#1620=EDGE_LOOP('',(#6251));
#1621=EDGE_LOOP('',(#6252));
#1622=EDGE_LOOP('',(#6253,#6254,#6255,#6256));
#1623=EDGE_LOOP('',(#6257));
#1624=EDGE_LOOP('',(#6258));
#1625=EDGE_LOOP('',(#6259,#6260,#6261,#6262));
#1626=EDGE_LOOP('',(#6263,#6264,#6265,#6266));
#1627=EDGE_LOOP('',(#6267,#6268,#6269,#6270,#6271,#6272,#6273,#6274));
#1628=EDGE_LOOP('',(#6275));
#1629=EDGE_LOOP('',(#6276));
#1630=EDGE_LOOP('',(#6277));
#1631=EDGE_LOOP('',(#6278));
#1632=EDGE_LOOP('',(#6279));
#1633=EDGE_LOOP('',(#6280,#6281,#6282,#6283));
#1634=EDGE_LOOP('',(#6284,#6285,#6286,#6287,#6288,#6289,#6290,#6291));
#1635=EDGE_LOOP('',(#6292));
#1636=EDGE_LOOP('',(#6293));
#1637=EDGE_LOOP('',(#6294));
#1638=EDGE_LOOP('',(#6295));
#1639=EDGE_LOOP('',(#6296));
#1640=EDGE_LOOP('',(#6297,#6298,#6299,#6300));
#1641=EDGE_LOOP('',(#6301,#6302,#6303,#6304));
#1642=EDGE_LOOP('',(#6305,#6306,#6307,#6308));
#1643=EDGE_LOOP('',(#6309));
#1644=EDGE_LOOP('',(#6310));
#1645=EDGE_LOOP('',(#6311));
#1646=EDGE_LOOP('',(#6312));
#1647=EDGE_LOOP('',(#6313,#6314,#6315,#6316));
#1648=EDGE_LOOP('',(#6317,#6318,#6319,#6320));
#1649=EDGE_LOOP('',(#6321));
#1650=EDGE_LOOP('',(#6322));
#1651=EDGE_LOOP('',(#6323));
#1652=EDGE_LOOP('',(#6324));
#1653=EDGE_LOOP('',(#6325,#6326,#6327,#6328));
#1654=EDGE_LOOP('',(#6329,#6330,#6331,#6332));
#1655=EDGE_LOOP('',(#6333));
#1656=EDGE_LOOP('',(#6334));
#1657=EDGE_LOOP('',(#6335));
#1658=EDGE_LOOP('',(#6336));
#1659=EDGE_LOOP('',(#6337,#6338,#6339,#6340));
#1660=EDGE_LOOP('',(#6341,#6342,#6343,#6344));
#1661=EDGE_LOOP('',(#6345));
#1662=EDGE_LOOP('',(#6346));
#1663=EDGE_LOOP('',(#6347));
#1664=EDGE_LOOP('',(#6348));
#1665=EDGE_LOOP('',(#6349,#6350,#6351,#6352));
#1666=EDGE_LOOP('',(#6353,#6354,#6355,#6356));
#1667=EDGE_LOOP('',(#6357));
#1668=EDGE_LOOP('',(#6358));
#1669=EDGE_LOOP('',(#6359));
#1670=EDGE_LOOP('',(#6360));
#1671=EDGE_LOOP('',(#6361,#6362,#6363,#6364));
#1672=EDGE_LOOP('',(#6365,#6366,#6367,#6368));
#1673=EDGE_LOOP('',(#6369));
#1674=EDGE_LOOP('',(#6370));
#1675=EDGE_LOOP('',(#6371));
#1676=EDGE_LOOP('',(#6372));
#1677=EDGE_LOOP('',(#6373,#6374,#6375,#6376));
#1678=EDGE_LOOP('',(#6377,#6378,#6379,#6380));
#1679=EDGE_LOOP('',(#6381,#6382,#6383,#6384));
#1680=EDGE_LOOP('',(#6385,#6386,#6387,#6388));
#1681=EDGE_LOOP('',(#6389,#6390,#6391,#6392,#6393,#6394,#6395,#6396));
#1682=EDGE_LOOP('',(#6397));
#1683=EDGE_LOOP('',(#6398,#6399,#6400,#6401));
#1684=EDGE_LOOP('',(#6402,#6403,#6404,#6405));
#1685=EDGE_LOOP('',(#6406,#6407,#6408,#6409));
#1686=EDGE_LOOP('',(#6410,#6411,#6412,#6413));
#1687=EDGE_LOOP('',(#6414,#6415,#6416,#6417));
#1688=EDGE_LOOP('',(#6418));
#1689=EDGE_LOOP('',(#6419));
#1690=EDGE_LOOP('',(#6420,#6421,#6422,#6423));
#1691=EDGE_LOOP('',(#6424,#6425,#6426,#6427,#6428,#6429,#6430,#6431));
#1692=EDGE_LOOP('',(#6432));
#1693=EDGE_LOOP('',(#6433,#6434,#6435,#6436));
#1694=EDGE_LOOP('',(#6437,#6438,#6439,#6440));
#1695=EDGE_LOOP('',(#6441,#6442,#6443,#6444));
#1696=EDGE_LOOP('',(#6445,#6446,#6447,#6448));
#1697=EDGE_LOOP('',(#6449,#6450,#6451,#6452,#6453,#6454,#6455,#6456));
#1698=EDGE_LOOP('',(#6457));
#1699=EDGE_LOOP('',(#6458,#6459,#6460,#6461));
#1700=EDGE_LOOP('',(#6462,#6463,#6464,#6465));
#1701=EDGE_LOOP('',(#6466,#6467,#6468,#6469));
#1702=EDGE_LOOP('',(#6470,#6471,#6472,#6473));
#1703=EDGE_LOOP('',(#6474,#6475,#6476,#6477));
#1704=EDGE_LOOP('',(#6478));
#1705=EDGE_LOOP('',(#6479));
#1706=EDGE_LOOP('',(#6480,#6481,#6482,#6483));
#1707=EDGE_LOOP('',(#6484,#6485,#6486,#6487,#6488,#6489,#6490,#6491));
#1708=EDGE_LOOP('',(#6492));
#1709=EDGE_LOOP('',(#6493,#6494,#6495,#6496));
#1710=EDGE_LOOP('',(#6497,#6498,#6499,#6500));
#1711=EDGE_LOOP('',(#6501,#6502,#6503,#6504));
#1712=EDGE_LOOP('',(#6505,#6506,#6507,#6508));
#1713=EDGE_LOOP('',(#6509,#6510,#6511,#6512));
#1714=EDGE_LOOP('',(#6513,#6514,#6515,#6516));
#1715=EDGE_LOOP('',(#6517,#6518,#6519,#6520));
#1716=EDGE_LOOP('',(#6521,#6522,#6523,#6524));
#1717=EDGE_LOOP('',(#6525,#6526,#6527,#6528));
#1718=EDGE_LOOP('',(#6529,#6530,#6531,#6532));
#1719=EDGE_LOOP('',(#6533,#6534,#6535,#6536));
#1720=EDGE_LOOP('',(#6537,#6538,#6539,#6540));
#1721=EDGE_LOOP('',(#6541,#6542,#6543,#6544,#6545,#6546));
#1722=EDGE_LOOP('',(#6547,#6548,#6549,#6550,#6551));
#1723=EDGE_LOOP('',(#6552,#6553,#6554,#6555));
#1724=EDGE_LOOP('',(#6556,#6557,#6558,#6559));
#1725=EDGE_LOOP('',(#6560));
#1726=EDGE_LOOP('',(#6561));
#1727=EDGE_LOOP('',(#6562,#6563,#6564,#6565,#6566));
#1728=EDGE_LOOP('',(#6567));
#1729=EDGE_LOOP('',(#6568));
#1730=EDGE_LOOP('',(#6569,#6570,#6571,#6572));
#1731=EDGE_LOOP('',(#6573,#6574,#6575,#6576,#6577,#6578));
#1732=EDGE_LOOP('',(#6579,#6580,#6581,#6582,#6583));
#1733=EDGE_LOOP('',(#6584));
#1734=EDGE_LOOP('',(#6585));
#1735=EDGE_LOOP('',(#6586,#6587,#6588,#6589));
#1736=EDGE_LOOP('',(#6590,#6591,#6592,#6593));
#1737=EDGE_LOOP('',(#6594,#6595,#6596,#6597));
#1738=EDGE_LOOP('',(#6598));
#1739=EDGE_LOOP('',(#6599));
#1740=EDGE_LOOP('',(#6600,#6601,#6602,#6603,#6604));
#1741=EDGE_LOOP('',(#6605,#6606));
#1742=EDGE_LOOP('',(#6607,#6608));
#1743=EDGE_LOOP('',(#6609,#6610));
#1744=EDGE_LOOP('',(#6611,#6612));
#1745=EDGE_LOOP('',(#6613,#6614));
#1746=EDGE_LOOP('',(#6615,#6616));
#1747=EDGE_LOOP('',(#6617,#6618));
#1748=EDGE_LOOP('',(#6619,#6620));
#1749=EDGE_LOOP('',(#6621,#6622,#6623,#6624));
#1750=EDGE_LOOP('',(#6625,#6626,#6627,#6628,#6629,#6630,#6631,#6632,#6633,
#6634,#6635,#6636,#6637,#6638,#6639,#6640,#6641,#6642,#6643,#6644));
#1751=EDGE_LOOP('',(#6645,#6646,#6647,#6648));
#1752=EDGE_LOOP('',(#6649,#6650,#6651,#6652));
#1753=EDGE_LOOP('',(#6653,#6654,#6655,#6656));
#1754=EDGE_LOOP('',(#6657,#6658,#6659,#6660));
#1755=EDGE_LOOP('',(#6661,#6662,#6663,#6664));
#1756=EDGE_LOOP('',(#6665,#6666,#6667,#6668,#6669,#6670));
#1757=EDGE_LOOP('',(#6671,#6672,#6673,#6674));
#1758=EDGE_LOOP('',(#6675,#6676,#6677,#6678));
#1759=EDGE_LOOP('',(#6679,#6680,#6681,#6682));
#1760=EDGE_LOOP('',(#6683,#6684,#6685,#6686));
#1761=EDGE_LOOP('',(#6687,#6688,#6689,#6690));
#1762=EDGE_LOOP('',(#6691,#6692,#6693,#6694));
#1763=EDGE_LOOP('',(#6695,#6696,#6697,#6698,#6699,#6700,#6701,#6702,#6703,
#6704,#6705,#6706,#6707,#6708,#6709,#6710,#6711,#6712,#6713,#6714));
#1764=EDGE_LOOP('',(#6715,#6716,#6717,#6718));
#1765=EDGE_LOOP('',(#6719,#6720,#6721,#6722));
#1766=EDGE_LOOP('',(#6723));
#1767=EDGE_LOOP('',(#6724));
#1768=EDGE_LOOP('',(#6725,#6726,#6727,#6728));
#1769=EDGE_LOOP('',(#6729));
#1770=EDGE_LOOP('',(#6730));
#1771=EDGE_LOOP('',(#6731,#6732,#6733,#6734));
#1772=EDGE_LOOP('',(#6735));
#1773=EDGE_LOOP('',(#6736));
#1774=EDGE_LOOP('',(#6737,#6738,#6739,#6740));
#1775=EDGE_LOOP('',(#6741));
#1776=EDGE_LOOP('',(#6742));
#1777=EDGE_LOOP('',(#6743,#6744,#6745,#6746));
#1778=EDGE_LOOP('',(#6747));
#1779=EDGE_LOOP('',(#6748));
#1780=EDGE_LOOP('',(#6749,#6750,#6751,#6752));
#1781=EDGE_LOOP('',(#6753,#6754,#6755,#6756));
#1782=EDGE_LOOP('',(#6757,#6758,#6759,#6760));
#1783=EDGE_LOOP('',(#6761,#6762,#6763,#6764));
#1784=EDGE_LOOP('',(#6765,#6766,#6767,#6768));
#1785=EDGE_LOOP('',(#6769,#6770,#6771,#6772));
#1786=EDGE_LOOP('',(#6773,#6774,#6775,#6776));
#1787=EDGE_LOOP('',(#6777,#6778,#6779,#6780,#6781,#6782));
#1788=EDGE_LOOP('',(#6783,#6784,#6785,#6786,#6787,#6788));
#1789=EDGE_LOOP('',(#6789));
#1790=EDGE_LOOP('',(#6790));
#1791=EDGE_LOOP('',(#6791,#6792,#6793,#6794));
#1792=EDGE_LOOP('',(#6795));
#1793=EDGE_LOOP('',(#6796));
#1794=EDGE_LOOP('',(#6797,#6798,#6799,#6800));
#1795=EDGE_LOOP('',(#6801,#6802,#6803,#6804));
#1796=EDGE_LOOP('',(#6805,#6806,#6807,#6808));
#1797=EDGE_LOOP('',(#6809));
#1798=EDGE_LOOP('',(#6810));
#1799=EDGE_LOOP('',(#6811,#6812,#6813,#6814));
#1800=EDGE_LOOP('',(#6815,#6816,#6817,#6818));
#1801=EDGE_LOOP('',(#6819,#6820,#6821,#6822));
#1802=EDGE_LOOP('',(#6823,#6824,#6825,#6826,#6827,#6828));
#1803=EDGE_LOOP('',(#6829,#6830,#6831,#6832,#6833));
#1804=EDGE_LOOP('',(#6834,#6835,#6836,#6837));
#1805=EDGE_LOOP('',(#6838,#6839,#6840,#6841));
#1806=EDGE_LOOP('',(#6842));
#1807=EDGE_LOOP('',(#6843));
#1808=EDGE_LOOP('',(#6844,#6845,#6846,#6847,#6848));
#1809=EDGE_LOOP('',(#6849));
#1810=EDGE_LOOP('',(#6850));
#1811=EDGE_LOOP('',(#6851,#6852,#6853,#6854));
#1812=EDGE_LOOP('',(#6855,#6856,#6857,#6858,#6859,#6860));
#1813=EDGE_LOOP('',(#6861,#6862,#6863,#6864,#6865));
#1814=EDGE_LOOP('',(#6866));
#1815=EDGE_LOOP('',(#6867));
#1816=EDGE_LOOP('',(#6868,#6869,#6870,#6871));
#1817=EDGE_LOOP('',(#6872,#6873,#6874,#6875));
#1818=EDGE_LOOP('',(#6876,#6877,#6878,#6879));
#1819=EDGE_LOOP('',(#6880));
#1820=EDGE_LOOP('',(#6881));
#1821=EDGE_LOOP('',(#6882,#6883,#6884,#6885,#6886));
#1822=EDGE_LOOP('',(#6887,#6888));
#1823=EDGE_LOOP('',(#6889,#6890));
#1824=EDGE_LOOP('',(#6891,#6892));
#1825=EDGE_LOOP('',(#6893,#6894));
#1826=EDGE_LOOP('',(#6895,#6896));
#1827=EDGE_LOOP('',(#6897,#6898));
#1828=EDGE_LOOP('',(#6899,#6900));
#1829=EDGE_LOOP('',(#6901,#6902,#6903,#6904));
#1830=EDGE_LOOP('',(#6905,#6906,#6907,#6908,#6909,#6910,#6911,#6912,#6913,
#6914,#6915,#6916,#6917,#6918,#6919,#6920,#6921,#6922));
#1831=EDGE_LOOP('',(#6923,#6924,#6925,#6926));
#1832=EDGE_LOOP('',(#6927,#6928,#6929,#6930));
#1833=EDGE_LOOP('',(#6931,#6932,#6933,#6934));
#1834=EDGE_LOOP('',(#6935,#6936,#6937,#6938));
#1835=EDGE_LOOP('',(#6939,#6940,#6941,#6942,#6943,#6944));
#1836=EDGE_LOOP('',(#6945,#6946,#6947,#6948));
#1837=EDGE_LOOP('',(#6949,#6950,#6951,#6952));
#1838=EDGE_LOOP('',(#6953,#6954,#6955,#6956));
#1839=EDGE_LOOP('',(#6957,#6958,#6959,#6960));
#1840=EDGE_LOOP('',(#6961,#6962,#6963,#6964));
#1841=EDGE_LOOP('',(#6965,#6966,#6967,#6968,#6969,#6970,#6971,#6972,#6973,
#6974,#6975,#6976,#6977,#6978,#6979,#6980,#6981,#6982));
#1842=EDGE_LOOP('',(#6983,#6984,#6985,#6986));
#1843=EDGE_LOOP('',(#6987,#6988,#6989,#6990));
#1844=EDGE_LOOP('',(#6991));
#1845=EDGE_LOOP('',(#6992));
#1846=EDGE_LOOP('',(#6993,#6994,#6995,#6996));
#1847=EDGE_LOOP('',(#6997));
#1848=EDGE_LOOP('',(#6998));
#1849=EDGE_LOOP('',(#6999,#7000,#7001,#7002));
#1850=EDGE_LOOP('',(#7003));
#1851=EDGE_LOOP('',(#7004));
#1852=EDGE_LOOP('',(#7005,#7006,#7007,#7008));
#1853=EDGE_LOOP('',(#7009));
#1854=EDGE_LOOP('',(#7010));
#1855=EDGE_LOOP('',(#7011,#7012,#7013,#7014));
#1856=EDGE_LOOP('',(#7015));
#1857=EDGE_LOOP('',(#7016));
#1858=EDGE_LOOP('',(#7017,#7018,#7019,#7020));
#1859=EDGE_LOOP('',(#7021,#7022,#7023,#7024));
#1860=EDGE_LOOP('',(#7025,#7026,#7027,#7028));
#1861=EDGE_LOOP('',(#7029,#7030,#7031,#7032));
#1862=EDGE_LOOP('',(#7033,#7034,#7035,#7036));
#1863=EDGE_LOOP('',(#7037,#7038,#7039,#7040));
#1864=EDGE_LOOP('',(#7041,#7042,#7043,#7044));
#1865=EDGE_LOOP('',(#7045,#7046,#7047,#7048,#7049,#7050));
#1866=EDGE_LOOP('',(#7051,#7052,#7053,#7054,#7055,#7056));
#1867=EDGE_LOOP('',(#7057));
#1868=EDGE_LOOP('',(#7058));
#1869=EDGE_LOOP('',(#7059,#7060,#7061,#7062));
#1870=EDGE_LOOP('',(#7063,#7064,#7065,#7066));
#1871=EDGE_LOOP('',(#7067,#7068,#7069,#7070));
#1872=EDGE_LOOP('',(#7071));
#1873=EDGE_LOOP('',(#7072));
#1874=EDGE_LOOP('',(#7073,#7074,#7075,#7076));
#1875=EDGE_LOOP('',(#7077,#7078,#7079,#7080));
#1876=EDGE_LOOP('',(#7081,#7082,#7083,#7084));
#1877=EDGE_LOOP('',(#7085));
#1878=EDGE_LOOP('',(#7086));
#1879=EDGE_LOOP('',(#7087));
#1880=EDGE_LOOP('',(#7088));
#1881=EDGE_LOOP('',(#7089));
#1882=EDGE_LOOP('',(#7090,#7091,#7092,#7093));
#1883=EDGE_LOOP('',(#7094,#7095,#7096,#7097));
#1884=EDGE_LOOP('',(#7098,#7099,#7100,#7101));
#1885=EDGE_LOOP('',(#7102));
#1886=EDGE_LOOP('',(#7103));
#1887=EDGE_LOOP('',(#7104,#7105,#7106,#7107));
#1888=EDGE_LOOP('',(#7108));
#1889=EDGE_LOOP('',(#7109));
#1890=EDGE_LOOP('',(#7110));
#1891=EDGE_LOOP('',(#7111,#7112,#7113,#7114));
#1892=EDGE_LOOP('',(#7115));
#1893=EDGE_LOOP('',(#7116));
#1894=EDGE_LOOP('',(#7117,#7118,#7119,#7120));
#1895=EDGE_LOOP('',(#7121,#7122,#7123,#7124));
#1896=EDGE_LOOP('',(#7125));
#1897=EDGE_LOOP('',(#7126));
#1898=EDGE_LOOP('',(#7127));
#1899=EDGE_LOOP('',(#7128));
#1900=EDGE_LOOP('',(#7129,#7130,#7131,#7132));
#1901=EDGE_LOOP('',(#7133,#7134,#7135,#7136));
#1902=EDGE_LOOP('',(#7137));
#1903=EDGE_LOOP('',(#7138));
#1904=EDGE_LOOP('',(#7139));
#1905=EDGE_LOOP('',(#7140));
#1906=EDGE_LOOP('',(#7141,#7142,#7143,#7144));
#1907=EDGE_LOOP('',(#7145));
#1908=EDGE_LOOP('',(#7146));
#1909=EDGE_LOOP('',(#7147,#7148,#7149,#7150));
#1910=EDGE_LOOP('',(#7151));
#1911=EDGE_LOOP('',(#7152));
#1912=EDGE_LOOP('',(#7153,#7154,#7155,#7156));
#1913=EDGE_LOOP('',(#7157,#7158,#7159,#7160));
#1914=EDGE_LOOP('',(#7161));
#1915=EDGE_LOOP('',(#7162));
#1916=EDGE_LOOP('',(#7163));
#1917=EDGE_LOOP('',(#7164));
#1918=EDGE_LOOP('',(#7165,#7166,#7167,#7168,#7169,#7170,#7171,#7172,#7173));
#1919=EDGE_LOOP('',(#7174,#7175,#7176,#7177,#7178,#7179,#7180));
#1920=EDGE_LOOP('',(#7181,#7182,#7183,#7184,#7185,#7186,#7187,#7188,#7189));
#1921=EDGE_LOOP('',(#7190,#7191,#7192));
#1922=EDGE_LOOP('',(#7193,#7194,#7195));
#1923=EDGE_LOOP('',(#7196,#7197,#7198));
#1924=EDGE_LOOP('',(#7199,#7200,#7201,#7202,#7203,#7204,#7205));
#1925=EDGE_LOOP('',(#7206,#7207,#7208,#7209,#7210,#7211,#7212));
#1926=EDGE_LOOP('',(#7213,#7214,#7215,#7216,#7217,#7218,#7219,#7220,#7221,
#7222));
#1927=EDGE_LOOP('',(#7223,#7224));
#1928=EDGE_LOOP('',(#7225,#7226));
#1929=EDGE_LOOP('',(#7227,#7228));
#1930=EDGE_LOOP('',(#7229));
#1931=EDGE_LOOP('',(#7230));
#1932=EDGE_LOOP('',(#7231));
#1933=EDGE_LOOP('',(#7232,#7233,#7234,#7235,#7236,#7237,#7238,#7239,#7240,
#7241,#7242,#7243,#7244,#7245,#7246,#7247,#7248,#7249,#7250,#7251,#7252,
#7253,#7254,#7255,#7256,#7257,#7258,#7259,#7260,#7261,#7262,#7263,#7264,
#7265,#7266,#7267,#7268,#7269,#7270,#7271));
#1934=EDGE_LOOP('',(#7272,#7273,#7274,#7275));
#1935=EDGE_LOOP('',(#7276));
#1936=EDGE_LOOP('',(#7277));
#1937=EDGE_LOOP('',(#7278));
#1938=EDGE_LOOP('',(#7279,#7280,#7281,#7282,#7283,#7284,#7285,#7286,#7287,
#7288,#7289,#7290,#7291,#7292,#7293,#7294,#7295,#7296,#7297,#7298,#7299,
#7300,#7301,#7302,#7303,#7304,#7305,#7306,#7307,#7308,#7309,#7310,#7311,
#7312,#7313,#7314,#7315,#7316,#7317,#7318));
#1939=EDGE_LOOP('',(#7319,#7320,#7321,#7322));
#1940=EDGE_LOOP('',(#7323));
#1941=EDGE_LOOP('',(#7324));
#1942=EDGE_LOOP('',(#7325,#7326,#7327,#7328));
#1943=EDGE_LOOP('',(#7329,#7330,#7331,#7332));
#1944=EDGE_LOOP('',(#7333,#7334,#7335,#7336));
#1945=EDGE_LOOP('',(#7337,#7338,#7339,#7340));
#1946=EDGE_LOOP('',(#7341,#7342,#7343,#7344));
#1947=EDGE_LOOP('',(#7345,#7346,#7347,#7348));
#1948=EDGE_LOOP('',(#7349,#7350,#7351,#7352));
#1949=EDGE_LOOP('',(#7353,#7354,#7355,#7356));
#1950=EDGE_LOOP('',(#7357,#7358,#7359,#7360));
#1951=EDGE_LOOP('',(#7361,#7362,#7363,#7364));
#1952=EDGE_LOOP('',(#7365,#7366,#7367,#7368));
#1953=EDGE_LOOP('',(#7369,#7370,#7371,#7372));
#1954=EDGE_LOOP('',(#7373,#7374,#7375,#7376));
#1955=EDGE_LOOP('',(#7377,#7378,#7379,#7380));
#1956=EDGE_LOOP('',(#7381,#7382,#7383,#7384));
#1957=EDGE_LOOP('',(#7385,#7386,#7387,#7388));
#1958=EDGE_LOOP('',(#7389,#7390,#7391,#7392));
#1959=EDGE_LOOP('',(#7393,#7394,#7395,#7396));
#1960=EDGE_LOOP('',(#7397,#7398,#7399,#7400));
#1961=EDGE_LOOP('',(#7401,#7402,#7403,#7404));
#1962=EDGE_LOOP('',(#7405,#7406,#7407,#7408));
#1963=EDGE_LOOP('',(#7409,#7410,#7411,#7412));
#1964=EDGE_LOOP('',(#7413,#7414,#7415,#7416));
#1965=EDGE_LOOP('',(#7417,#7418,#7419,#7420));
#1966=EDGE_LOOP('',(#7421,#7422,#7423,#7424));
#1967=EDGE_LOOP('',(#7425,#7426,#7427,#7428));
#1968=EDGE_LOOP('',(#7429,#7430,#7431,#7432));
#1969=EDGE_LOOP('',(#7433,#7434,#7435,#7436));
#1970=EDGE_LOOP('',(#7437,#7438,#7439,#7440));
#1971=EDGE_LOOP('',(#7441,#7442,#7443,#7444));
#1972=EDGE_LOOP('',(#7445,#7446,#7447,#7448));
#1973=EDGE_LOOP('',(#7449,#7450,#7451,#7452));
#1974=EDGE_LOOP('',(#7453,#7454,#7455,#7456));
#1975=EDGE_LOOP('',(#7457,#7458,#7459,#7460));
#1976=EDGE_LOOP('',(#7461,#7462,#7463,#7464));
#1977=EDGE_LOOP('',(#7465,#7466,#7467,#7468));
#1978=EDGE_LOOP('',(#7469,#7470,#7471,#7472));
#1979=EDGE_LOOP('',(#7473,#7474,#7475,#7476));
#1980=EDGE_LOOP('',(#7477,#7478,#7479,#7480));
#1981=EDGE_LOOP('',(#7481,#7482,#7483,#7484));
#1982=EDGE_LOOP('',(#7485,#7486,#7487,#7488));
#1983=EDGE_LOOP('',(#7489));
#1984=EDGE_LOOP('',(#7490));
#1985=EDGE_LOOP('',(#7491));
#1986=EDGE_LOOP('',(#7492));
#1987=EDGE_LOOP('',(#7493));
#1988=EDGE_LOOP('',(#7494,#7495,#7496,#7497));
#1989=EDGE_LOOP('',(#7498,#7499,#7500,#7501));
#1990=EDGE_LOOP('',(#7502));
#1991=EDGE_LOOP('',(#7503));
#1992=EDGE_LOOP('',(#7504,#7505,#7506,#7507));
#1993=EDGE_LOOP('',(#7508));
#1994=EDGE_LOOP('',(#7509,#7510,#7511,#7512));
#1995=EDGE_LOOP('',(#7513,#7514,#7515,#7516));
#1996=EDGE_LOOP('',(#7517));
#1997=EDGE_LOOP('',(#7518));
#1998=EDGE_LOOP('',(#7519));
#1999=EDGE_LOOP('',(#7520));
#2000=EDGE_LOOP('',(#7521,#7522,#7523,#7524));
#2001=EDGE_LOOP('',(#7525,#7526,#7527,#7528));
#2002=EDGE_LOOP('',(#7529));
#2003=EDGE_LOOP('',(#7530));
#2004=EDGE_LOOP('',(#7531));
#2005=EDGE_LOOP('',(#7532));
#2006=EDGE_LOOP('',(#7533,#7534,#7535,#7536));
#2007=EDGE_LOOP('',(#7537));
#2008=EDGE_LOOP('',(#7538));
#2009=EDGE_LOOP('',(#7539,#7540,#7541,#7542));
#2010=EDGE_LOOP('',(#7543));
#2011=EDGE_LOOP('',(#7544));
#2012=EDGE_LOOP('',(#7545,#7546,#7547,#7548));
#2013=EDGE_LOOP('',(#7549,#7550,#7551,#7552));
#2014=EDGE_LOOP('',(#7553));
#2015=EDGE_LOOP('',(#7554));
#2016=EDGE_LOOP('',(#7555));
#2017=EDGE_LOOP('',(#7556));
#2018=EDGE_LOOP('',(#7557,#7558,#7559,#7560,#7561,#7562,#7563,#7564,#7565));
#2019=EDGE_LOOP('',(#7566,#7567,#7568,#7569,#7570,#7571,#7572));
#2020=EDGE_LOOP('',(#7573,#7574,#7575,#7576,#7577,#7578,#7579,#7580,#7581));
#2021=EDGE_LOOP('',(#7582,#7583,#7584));
#2022=EDGE_LOOP('',(#7585,#7586,#7587));
#2023=EDGE_LOOP('',(#7588,#7589,#7590));
#2024=EDGE_LOOP('',(#7591,#7592,#7593,#7594,#7595,#7596,#7597));
#2025=EDGE_LOOP('',(#7598,#7599,#7600,#7601,#7602,#7603,#7604));
#2026=EDGE_LOOP('',(#7605,#7606,#7607,#7608,#7609,#7610,#7611,#7612,#7613,
#7614));
#2027=EDGE_LOOP('',(#7615,#7616));
#2028=EDGE_LOOP('',(#7617,#7618));
#2029=EDGE_LOOP('',(#7619,#7620));
#2030=EDGE_LOOP('',(#7621));
#2031=EDGE_LOOP('',(#7622));
#2032=EDGE_LOOP('',(#7623));
#2033=EDGE_LOOP('',(#7624,#7625,#7626,#7627,#7628,#7629,#7630,#7631,#7632,
#7633,#7634,#7635,#7636,#7637,#7638,#7639,#7640,#7641,#7642,#7643,#7644,
#7645,#7646,#7647,#7648,#7649,#7650,#7651,#7652,#7653,#7654,#7655,#7656,
#7657,#7658,#7659,#7660,#7661,#7662,#7663,#7664,#7665,#7666,#7667,#7668,
#7669,#7670,#7671,#7672,#7673,#7674,#7675,#7676,#7677,#7678,#7679,#7680,
#7681,#7682,#7683,#7684,#7685,#7686,#7687,#7688,#7689,#7690,#7691,#7692,
#7693,#7694,#7695,#7696,#7697,#7698,#7699,#7700,#7701,#7702,#7703));
#2034=EDGE_LOOP('',(#7704,#7705,#7706,#7707));
#2035=EDGE_LOOP('',(#7708));
#2036=EDGE_LOOP('',(#7709));
#2037=EDGE_LOOP('',(#7710));
#2038=EDGE_LOOP('',(#7711,#7712,#7713,#7714,#7715,#7716,#7717,#7718,#7719,
#7720,#7721,#7722,#7723,#7724,#7725,#7726,#7727,#7728,#7729,#7730,#7731,
#7732,#7733,#7734,#7735,#7736,#7737,#7738,#7739,#7740,#7741,#7742,#7743,
#7744,#7745,#7746,#7747,#7748,#7749,#7750,#7751,#7752,#7753,#7754,#7755,
#7756,#7757,#7758,#7759,#7760,#7761,#7762,#7763,#7764,#7765,#7766,#7767,
#7768,#7769,#7770,#7771,#7772,#7773,#7774,#7775,#7776,#7777,#7778,#7779,
#7780,#7781,#7782,#7783,#7784,#7785,#7786,#7787,#7788,#7789,#7790));
#2039=EDGE_LOOP('',(#7791,#7792,#7793,#7794));
#2040=EDGE_LOOP('',(#7795));
#2041=EDGE_LOOP('',(#7796));
#2042=EDGE_LOOP('',(#7797,#7798,#7799,#7800));
#2043=EDGE_LOOP('',(#7801,#7802,#7803,#7804));
#2044=EDGE_LOOP('',(#7805,#7806,#7807,#7808));
#2045=EDGE_LOOP('',(#7809,#7810,#7811,#7812));
#2046=EDGE_LOOP('',(#7813,#7814,#7815,#7816));
#2047=EDGE_LOOP('',(#7817,#7818,#7819,#7820));
#2048=EDGE_LOOP('',(#7821,#7822,#7823,#7824));
#2049=EDGE_LOOP('',(#7825,#7826,#7827,#7828));
#2050=EDGE_LOOP('',(#7829,#7830,#7831,#7832));
#2051=EDGE_LOOP('',(#7833,#7834,#7835,#7836));
#2052=EDGE_LOOP('',(#7837,#7838,#7839,#7840));
#2053=EDGE_LOOP('',(#7841,#7842,#7843,#7844));
#2054=EDGE_LOOP('',(#7845,#7846,#7847,#7848));
#2055=EDGE_LOOP('',(#7849,#7850,#7851,#7852));
#2056=EDGE_LOOP('',(#7853,#7854,#7855,#7856));
#2057=EDGE_LOOP('',(#7857,#7858,#7859,#7860));
#2058=EDGE_LOOP('',(#7861,#7862,#7863,#7864));
#2059=EDGE_LOOP('',(#7865,#7866,#7867,#7868));
#2060=EDGE_LOOP('',(#7869,#7870,#7871,#7872));
#2061=EDGE_LOOP('',(#7873,#7874,#7875,#7876));
#2062=EDGE_LOOP('',(#7877,#7878,#7879,#7880));
#2063=EDGE_LOOP('',(#7881,#7882,#7883,#7884));
#2064=EDGE_LOOP('',(#7885,#7886,#7887,#7888));
#2065=EDGE_LOOP('',(#7889,#7890,#7891,#7892));
#2066=EDGE_LOOP('',(#7893,#7894,#7895,#7896));
#2067=EDGE_LOOP('',(#7897,#7898,#7899,#7900));
#2068=EDGE_LOOP('',(#7901,#7902,#7903,#7904));
#2069=EDGE_LOOP('',(#7905,#7906,#7907,#7908));
#2070=EDGE_LOOP('',(#7909,#7910,#7911,#7912));
#2071=EDGE_LOOP('',(#7913,#7914,#7915,#7916));
#2072=EDGE_LOOP('',(#7917,#7918,#7919,#7920));
#2073=EDGE_LOOP('',(#7921,#7922,#7923,#7924));
#2074=EDGE_LOOP('',(#7925,#7926,#7927,#7928));
#2075=EDGE_LOOP('',(#7929,#7930,#7931,#7932));
#2076=EDGE_LOOP('',(#7933,#7934,#7935,#7936));
#2077=EDGE_LOOP('',(#7937,#7938,#7939,#7940));
#2078=EDGE_LOOP('',(#7941,#7942,#7943,#7944));
#2079=EDGE_LOOP('',(#7945,#7946,#7947,#7948));
#2080=EDGE_LOOP('',(#7949,#7950,#7951,#7952));
#2081=EDGE_LOOP('',(#7953,#7954,#7955,#7956));
#2082=EDGE_LOOP('',(#7957,#7958,#7959,#7960));
#2083=EDGE_LOOP('',(#7961,#7962,#7963,#7964));
#2084=EDGE_LOOP('',(#7965,#7966,#7967,#7968));
#2085=EDGE_LOOP('',(#7969,#7970,#7971,#7972));
#2086=EDGE_LOOP('',(#7973,#7974,#7975,#7976));
#2087=EDGE_LOOP('',(#7977,#7978,#7979,#7980));
#2088=EDGE_LOOP('',(#7981,#7982,#7983,#7984));
#2089=EDGE_LOOP('',(#7985,#7986,#7987,#7988));
#2090=EDGE_LOOP('',(#7989,#7990,#7991,#7992));
#2091=EDGE_LOOP('',(#7993,#7994,#7995,#7996));
#2092=EDGE_LOOP('',(#7997,#7998,#7999,#8000));
#2093=EDGE_LOOP('',(#8001,#8002,#8003,#8004));
#2094=EDGE_LOOP('',(#8005,#8006,#8007,#8008));
#2095=EDGE_LOOP('',(#8009,#8010,#8011,#8012));
#2096=EDGE_LOOP('',(#8013,#8014,#8015,#8016));
#2097=EDGE_LOOP('',(#8017,#8018,#8019,#8020));
#2098=EDGE_LOOP('',(#8021,#8022,#8023,#8024));
#2099=EDGE_LOOP('',(#8025,#8026,#8027,#8028));
#2100=EDGE_LOOP('',(#8029,#8030,#8031,#8032));
#2101=EDGE_LOOP('',(#8033,#8034,#8035,#8036));
#2102=EDGE_LOOP('',(#8037,#8038,#8039,#8040));
#2103=EDGE_LOOP('',(#8041,#8042,#8043,#8044));
#2104=EDGE_LOOP('',(#8045,#8046,#8047,#8048));
#2105=EDGE_LOOP('',(#8049,#8050,#8051,#8052));
#2106=EDGE_LOOP('',(#8053,#8054,#8055,#8056));
#2107=EDGE_LOOP('',(#8057,#8058,#8059,#8060));
#2108=EDGE_LOOP('',(#8061,#8062,#8063,#8064));
#2109=EDGE_LOOP('',(#8065,#8066,#8067,#8068));
#2110=EDGE_LOOP('',(#8069,#8070,#8071,#8072));
#2111=EDGE_LOOP('',(#8073,#8074,#8075,#8076));
#2112=EDGE_LOOP('',(#8077,#8078,#8079,#8080));
#2113=EDGE_LOOP('',(#8081,#8082,#8083,#8084));
#2114=EDGE_LOOP('',(#8085,#8086,#8087,#8088));
#2115=EDGE_LOOP('',(#8089,#8090,#8091,#8092));
#2116=EDGE_LOOP('',(#8093,#8094,#8095,#8096));
#2117=EDGE_LOOP('',(#8097,#8098,#8099,#8100));
#2118=EDGE_LOOP('',(#8101,#8102,#8103,#8104));
#2119=EDGE_LOOP('',(#8105,#8106,#8107,#8108));
#2120=EDGE_LOOP('',(#8109,#8110,#8111,#8112));
#2121=EDGE_LOOP('',(#8113,#8114,#8115,#8116));
#2122=EDGE_LOOP('',(#8117));
#2123=EDGE_LOOP('',(#8118,#8119,#8120,#8121));
#2124=EDGE_LOOP('',(#8122,#8123,#8124,#8125));
#2125=EDGE_LOOP('',(#8126,#8127,#8128,#8129));
#2126=EDGE_LOOP('',(#8130));
#2127=EDGE_LOOP('',(#8131));
#2128=EDGE_LOOP('',(#8132,#8133,#8134,#8135));
#2129=EDGE_LOOP('',(#8136,#8137,#8138,#8139));
#2130=EDGE_LOOP('',(#8140,#8141,#8142,#8143));
#2131=EDGE_LOOP('',(#8144));
#2132=EDGE_LOOP('',(#8145,#8146,#8147,#8148));
#2133=EDGE_LOOP('',(#8149,#8150,#8151,#8152));
#2134=EDGE_LOOP('',(#8153,#8154,#8155,#8156));
#2135=EDGE_LOOP('',(#8157,#8158,#8159,#8160));
#2136=EDGE_LOOP('',(#8161,#8162,#8163,#8164));
#2137=EDGE_LOOP('',(#8165,#8166,#8167,#8168));
#2138=EDGE_LOOP('',(#8169,#8170,#8171,#8172,#8173,#8174));
#2139=EDGE_LOOP('',(#8175,#8176,#8177,#8178,#8179,#8180));
#2140=CIRCLE('',#9520,0.225);
#2141=CIRCLE('',#9521,0.225);
#2142=CIRCLE('',#9523,0.225);
#2143=CIRCLE('',#9524,0.225);
#2144=CIRCLE('',#9526,0.225);
#2145=CIRCLE('',#9527,0.225);
#2146=CIRCLE('',#9528,0.225);
#2147=CIRCLE('',#9529,0.225);
#2148=CIRCLE('',#9530,0.225);
#2149=CIRCLE('',#9531,0.225);
#2150=CIRCLE('',#9535,0.225);
#2151=CIRCLE('',#9537,0.225);
#2152=CIRCLE('',#9541,0.225);
#2153=CIRCLE('',#9542,0.225);
#2154=CIRCLE('',#9543,0.225);
#2155=CIRCLE('',#9545,0.225);
#2156=CIRCLE('',#9549,0.225);
#2157=CIRCLE('',#9550,0.225);
#2158=CIRCLE('',#9551,0.225);
#2159=CIRCLE('',#9553,0.225);
#2160=CIRCLE('',#9557,0.165);
#2161=CIRCLE('',#9558,0.165);
#2162=CIRCLE('',#9561,0.165);
#2163=CIRCLE('',#9562,0.165);
#2164=CIRCLE('',#9565,0.165);
#2165=CIRCLE('',#9566,0.165);
#2166=CIRCLE('',#9569,0.165);
#2167=CIRCLE('',#9570,0.165);
#2168=CIRCLE('',#9593,0.165);
#2169=CIRCLE('',#9594,0.165);
#2170=CIRCLE('',#9596,0.165);
#2171=CIRCLE('',#9597,0.165);
#2172=CIRCLE('',#9599,0.165);
#2173=CIRCLE('',#9600,0.165);
#2174=CIRCLE('',#9602,0.165);
#2175=CIRCLE('',#9603,0.165);
#2176=CIRCLE('',#9605,1.5);
#2177=CIRCLE('',#9606,1.5);
#2178=CIRCLE('',#9608,0.225);
#2179=CIRCLE('',#9609,0.225);
#2180=CIRCLE('',#9611,0.225);
#2181=CIRCLE('',#9612,0.225);
#2182=CIRCLE('',#9614,0.225);
#2183=CIRCLE('',#9615,0.225);
#2184=CIRCLE('',#9617,0.225);
#2185=CIRCLE('',#9618,0.225);
#2186=CIRCLE('',#9631,1.1);
#2187=CIRCLE('',#9632,1.1);
#2188=CIRCLE('',#9634,1.49);
#2189=CIRCLE('',#9635,1.49);
#2190=CIRCLE('',#9640,0.225);
#2191=CIRCLE('',#9641,0.225);
#2192=CIRCLE('',#9643,0.225);
#2193=CIRCLE('',#9644,0.225);
#2194=CIRCLE('',#9646,0.225);
#2195=CIRCLE('',#9647,0.225);
#2196=CIRCLE('',#9649,0.225);
#2197=CIRCLE('',#9650,0.225);
#2198=CIRCLE('',#9652,2.1);
#2199=CIRCLE('',#9653,2.1);
#2200=CIRCLE('',#9654,2.1);
#2201=CIRCLE('',#9655,2.1);
#2202=CIRCLE('',#9656,1.1);
#2203=CIRCLE('',#9658,2.1);
#2204=CIRCLE('',#9660,2.1);
#2205=CIRCLE('',#9662,2.1);
#2206=CIRCLE('',#9664,2.1);
#2207=CIRCLE('',#9666,1.49);
#2208=CIRCLE('',#9667,1.49);
#2209=CIRCLE('',#9669,1.1);
#2210=CIRCLE('',#9674,0.225);
#2211=CIRCLE('',#9675,0.225);
#2212=CIRCLE('',#9677,0.225);
#2213=CIRCLE('',#9678,0.225);
#2214=CIRCLE('',#9680,0.225);
#2215=CIRCLE('',#9681,0.225);
#2216=CIRCLE('',#9683,0.225);
#2217=CIRCLE('',#9684,0.225);
#2218=CIRCLE('',#9686,2.1);
#2219=CIRCLE('',#9687,2.1);
#2220=CIRCLE('',#9688,2.1);
#2221=CIRCLE('',#9689,2.1);
#2222=CIRCLE('',#9690,1.49);
#2223=CIRCLE('',#9692,2.1);
#2224=CIRCLE('',#9694,2.1);
#2225=CIRCLE('',#9696,2.1);
#2226=CIRCLE('',#9698,2.1);
#2227=CIRCLE('',#9700,1.49);
#2228=CIRCLE('',#9702,1.1);
#2229=CIRCLE('',#9704,1.1);
#2230=CIRCLE('',#9708,0.165);
#2231=CIRCLE('',#9709,0.165);
#2232=CIRCLE('',#9711,0.165);
#2233=CIRCLE('',#9712,0.165);
#2234=CIRCLE('',#9714,0.164999999999999);
#2235=CIRCLE('',#9715,0.164999999999999);
#2236=CIRCLE('',#9717,0.164999999999999);
#2237=CIRCLE('',#9718,0.164999999999999);
#2238=CIRCLE('',#9720,1.6);
#2239=CIRCLE('',#9721,1.6);
#2240=CIRCLE('',#9723,0.225);
#2241=CIRCLE('',#9724,0.225);
#2242=CIRCLE('',#9726,0.225);
#2243=CIRCLE('',#9727,0.225);
#2244=CIRCLE('',#9729,0.225);
#2245=CIRCLE('',#9730,0.225);
#2246=CIRCLE('',#9732,0.225);
#2247=CIRCLE('',#9733,0.225);
#2248=CIRCLE('',#9746,0.165);
#2249=CIRCLE('',#9747,0.165);
#2250=CIRCLE('',#9749,0.4);
#2251=CIRCLE('',#9750,0.4);
#2252=CIRCLE('',#9755,0.165);
#2253=CIRCLE('',#9756,0.165);
#2254=CIRCLE('',#9758,0.4);
#2255=CIRCLE('',#9759,0.4);
#2256=CIRCLE('',#9764,0.164999999999999);
#2257=CIRCLE('',#9765,0.164999999999999);
#2258=CIRCLE('',#9767,0.4);
#2259=CIRCLE('',#9768,0.4);
#2260=CIRCLE('',#9773,0.164999999999999);
#2261=CIRCLE('',#9774,0.164999999999999);
#2262=CIRCLE('',#9776,0.4);
#2263=CIRCLE('',#9777,0.4);
#2264=CIRCLE('',#9782,1.2);
#2265=CIRCLE('',#9783,1.2);
#2266=CIRCLE('',#9785,1.59);
#2267=CIRCLE('',#9786,1.59);
#2268=CIRCLE('',#9791,0.225);
#2269=CIRCLE('',#9792,0.225);
#2270=CIRCLE('',#9794,0.225);
#2271=CIRCLE('',#9795,0.225);
#2272=CIRCLE('',#9797,0.225);
#2273=CIRCLE('',#9798,0.225);
#2274=CIRCLE('',#9800,0.225);
#2275=CIRCLE('',#9801,0.225);
#2276=CIRCLE('',#9803,2.2);
#2277=CIRCLE('',#9804,2.2);
#2278=CIRCLE('',#9805,2.2);
#2279=CIRCLE('',#9806,2.2);
#2280=CIRCLE('',#9807,1.2);
#2281=CIRCLE('',#9809,2.2);
#2282=CIRCLE('',#9811,2.2);
#2283=CIRCLE('',#9813,2.2);
#2284=CIRCLE('',#9815,2.2);
#2285=CIRCLE('',#9817,1.59);
#2286=CIRCLE('',#9818,1.59);
#2287=CIRCLE('',#9820,1.2);
#2288=CIRCLE('',#9825,0.225);
#2289=CIRCLE('',#9826,0.225);
#2290=CIRCLE('',#9828,0.225);
#2291=CIRCLE('',#9829,0.225);
#2292=CIRCLE('',#9831,0.225);
#2293=CIRCLE('',#9832,0.225);
#2294=CIRCLE('',#9834,0.225);
#2295=CIRCLE('',#9835,0.225);
#2296=CIRCLE('',#9837,2.2);
#2297=CIRCLE('',#9838,2.2);
#2298=CIRCLE('',#9839,2.2);
#2299=CIRCLE('',#9840,2.2);
#2300=CIRCLE('',#9841,1.59);
#2301=CIRCLE('',#9843,2.2);
#2302=CIRCLE('',#9845,2.2);
#2303=CIRCLE('',#9847,2.2);
#2304=CIRCLE('',#9849,2.2);
#2305=CIRCLE('',#9851,1.59);
#2306=CIRCLE('',#9853,1.2);
#2307=CIRCLE('',#9855,1.2);
#2308=CIRCLE('',#9861,0.736619772367581);
#2309=CIRCLE('',#9862,1.37323954473516);
#2310=CIRCLE('',#9863,0.636619772367581);
#2311=CIRCLE('',#9864,1.27323954473516);
#2312=CIRCLE('',#9866,0.636619772367581);
#2313=CIRCLE('',#9868,1.27323954473516);
#2314=CIRCLE('',#9870,1.37323954473516);
#2315=CIRCLE('',#9874,0.736619772367581);
#2316=CIRCLE('',#9879,0.976185);
#2317=CIRCLE('',#9880,0.976185);
#2318=CIRCLE('',#9881,0.247676);
#2319=CIRCLE('',#9882,0.976185);
#2320=CIRCLE('',#9883,0.976185);
#2321=CIRCLE('',#9885,0.976185);
#2322=CIRCLE('',#9887,0.5);
#2323=CIRCLE('',#9888,0.5);
#2324=CIRCLE('',#9890,0.56);
#2325=CIRCLE('',#9893,0.976185);
#2326=CIRCLE('',#9895,0.56);
#2327=CIRCLE('',#9899,1.023815);
#2328=CIRCLE('',#9900,1.023815);
#2329=CIRCLE('',#9901,0.247676);
#2330=CIRCLE('',#9902,1.023815);
#2331=CIRCLE('',#9903,1.023815);
#2332=CIRCLE('',#9905,1.023815);
#2333=CIRCLE('',#9907,1.44);
#2334=CIRCLE('',#9908,1.023815);
#2335=CIRCLE('',#9910,1.5);
#2336=CIRCLE('',#9912,1.5);
#2337=CIRCLE('',#9914,1.44);
#2338=CIRCLE('',#9919,0.23815);
#2339=CIRCLE('',#9921,0.23815);
#2340=CIRCLE('',#9923,0.23815);
#2341=CIRCLE('',#9925,0.23815);
#2342=CIRCLE('',#9927,0.23815);
#2343=CIRCLE('',#9929,0.23815);
#2344=CIRCLE('',#9931,0.23815);
#2345=CIRCLE('',#9933,0.23815);
#2346=CIRCLE('',#9936,0.243053047864041);
#2347=CIRCLE('',#9937,0.243053047864041);
#2348=CIRCLE('',#9939,1.019052);
#2349=CIRCLE('',#9940,1.019052);
#2350=CIRCLE('',#9941,1.019052);
#2351=CIRCLE('',#9942,1.019052);
#2352=CIRCLE('',#9943,1.019052);
#2353=CIRCLE('',#9944,1.019052);
#2354=CIRCLE('',#9945,1.019052);
#2355=CIRCLE('',#9946,1.019052);
#2356=CIRCLE('',#9947,1.019052);
#2357=CIRCLE('',#9949,0.980948);
#2358=CIRCLE('',#9950,0.243053047864041);
#2359=CIRCLE('',#9952,0.243053047864041);
#2360=CIRCLE('',#9954,0.980948);
#2361=CIRCLE('',#9955,0.243053047864041);
#2362=CIRCLE('',#9957,0.243053047864041);
#2363=CIRCLE('',#9959,0.980948);
#2364=CIRCLE('',#9960,0.243053047864041);
#2365=CIRCLE('',#9962,0.243053047864041);
#2366=CIRCLE('',#9964,0.980948);
#2367=CIRCLE('',#9965,0.243053047864041);
#2368=CIRCLE('',#9967,0.243053047864041);
#2369=CIRCLE('',#9969,0.980948);
#2370=CIRCLE('',#9970,0.243053047864041);
#2371=CIRCLE('',#9972,0.243053047864041);
#2372=CIRCLE('',#9974,0.980948);
#2373=CIRCLE('',#9975,0.243053047864041);
#2374=CIRCLE('',#9977,0.243053047864041);
#2375=CIRCLE('',#9979,0.980948);
#2376=CIRCLE('',#9980,0.980948);
#2377=CIRCLE('',#9981,0.980948);
#2378=CIRCLE('',#9983,0.243053047864041);
#2379=CIRCLE('',#9985,0.243053047864041);
#2380=CIRCLE('',#9990,1.013815);
#2381=CIRCLE('',#9991,0.991185);
#2382=CIRCLE('',#9993,1.013815);
#2383=CIRCLE('',#9995,0.991185);
#2384=CIRCLE('',#9998,1.013815);
#2385=CIRCLE('',#9999,0.991185);
#2386=CIRCLE('',#10001,1.013815);
#2387=CIRCLE('',#10003,0.991185);
#2388=CIRCLE('',#10020,0.2);
#2389=CIRCLE('',#10021,0.16);
#2390=CIRCLE('',#10023,0.2);
#2391=CIRCLE('',#10026,0.3);
#2392=CIRCLE('',#10028,0.35);
#2393=CIRCLE('',#10030,0.35);
#2394=CIRCLE('',#10032,0.32);
#2395=CIRCLE('',#10034,0.22);
#2396=CIRCLE('',#10036,0.1954);
#2397=CIRCLE('',#10038,0.1954);
#2398=CIRCLE('',#10043,1.070235);
#2399=CIRCLE('',#10044,1.070235);
#2400=CIRCLE('',#10045,0.309556);
#2401=CIRCLE('',#10046,1.070235);
#2402=CIRCLE('',#10047,1.070235);
#2403=CIRCLE('',#10049,1.070235);
#2404=CIRCLE('',#10051,0.6);
#2405=CIRCLE('',#10052,0.6);
#2406=CIRCLE('',#10054,0.66);
#2407=CIRCLE('',#10057,1.070235);
#2408=CIRCLE('',#10059,0.66);
#2409=CIRCLE('',#10063,1.129765);
#2410=CIRCLE('',#10064,1.129765);
#2411=CIRCLE('',#10065,0.309556);
#2412=CIRCLE('',#10066,1.129765);
#2413=CIRCLE('',#10067,1.129765);
#2414=CIRCLE('',#10069,1.129765);
#2415=CIRCLE('',#10071,1.54);
#2416=CIRCLE('',#10072,1.129765);
#2417=CIRCLE('',#10074,1.6);
#2418=CIRCLE('',#10076,1.6);
#2419=CIRCLE('',#10078,1.54);
#2420=CIRCLE('',#10083,0.29765);
#2421=CIRCLE('',#10085,0.29765);
#2422=CIRCLE('',#10087,0.29765);
#2423=CIRCLE('',#10089,0.29765);
#2424=CIRCLE('',#10091,0.29765);
#2425=CIRCLE('',#10093,0.29765);
#2426=CIRCLE('',#10095,0.29765);
#2427=CIRCLE('',#10098,0.303778037777585);
#2428=CIRCLE('',#10099,0.303778037777585);
#2429=CIRCLE('',#10101,1.123812);
#2430=CIRCLE('',#10102,1.123812);
#2431=CIRCLE('',#10103,1.123812);
#2432=CIRCLE('',#10104,1.123812);
#2433=CIRCLE('',#10105,1.123812);
#2434=CIRCLE('',#10106,1.123812);
#2435=CIRCLE('',#10107,1.123812);
#2436=CIRCLE('',#10108,1.123812);
#2437=CIRCLE('',#10109,1.123812);
#2438=CIRCLE('',#10111,1.076188);
#2439=CIRCLE('',#10112,0.303778037777585);
#2440=CIRCLE('',#10114,0.303778037777585);
#2441=CIRCLE('',#10116,1.076188);
#2442=CIRCLE('',#10117,0.303778037777585);
#2443=CIRCLE('',#10119,0.303778037777585);
#2444=CIRCLE('',#10121,1.076188);
#2445=CIRCLE('',#10122,1.076188);
#2446=CIRCLE('',#10123,0.303778037777585);
#2447=CIRCLE('',#10125,0.303778037777585);
#2448=CIRCLE('',#10127,1.076188);
#2449=CIRCLE('',#10128,0.303778037777585);
#2450=CIRCLE('',#10130,0.303778037777585);
#2451=CIRCLE('',#10132,1.076188);
#2452=CIRCLE('',#10133,0.303778037777585);
#2453=CIRCLE('',#10135,0.303778037777585);
#2454=CIRCLE('',#10137,1.076188);
#2455=CIRCLE('',#10138,1.076188);
#2456=CIRCLE('',#10139,1.076188);
#2457=CIRCLE('',#10141,0.303778037777585);
#2458=CIRCLE('',#10143,0.303778037777585);
#2459=CIRCLE('',#10148,1.119765);
#2460=CIRCLE('',#10149,1.085235);
#2461=CIRCLE('',#10151,1.119765);
#2462=CIRCLE('',#10153,1.085235);
#2463=CIRCLE('',#10156,1.119765);
#2464=CIRCLE('',#10157,1.085235);
#2465=CIRCLE('',#10159,1.119765);
#2466=CIRCLE('',#10161,1.085235);
#2467=CIRCLE('',#10178,0.1954);
#2468=CIRCLE('',#10180,0.3);
#2469=CIRCLE('',#10182,0.35);
#2470=CIRCLE('',#10184,0.35);
#2471=CIRCLE('',#10186,0.32);
#2472=CIRCLE('',#10188,0.22);
#2473=CIRCLE('',#10190,0.1954);
#2474=CIRCLE('',#10195,0.165);
#2475=CIRCLE('',#10196,0.165);
#2476=CIRCLE('',#10199,0.7);
#2477=CIRCLE('',#10200,0.5);
#2478=CIRCLE('',#10202,0.7);
#2479=CIRCLE('',#10203,0.5);
#2480=CIRCLE('',#10206,0.5);
#2481=CIRCLE('',#10208,0.4);
#2482=CIRCLE('',#10209,0.4);
#2483=CIRCLE('',#10212,0.5);
#2484=CIRCLE('',#10217,0.505);
#2485=CIRCLE('',#10218,0.505);
#2486=CIRCLE('',#10220,0.405);
#2487=CIRCLE('',#10222,0.405);
#2488=CIRCLE('',#10224,0.7);
#2489=CIRCLE('',#10225,0.7);
#2490=CIRCLE('',#10230,0.505);
#2491=CIRCLE('',#10231,0.505);
#2492=CIRCLE('',#10233,0.7);
#2493=CIRCLE('',#10234,0.7);
#2494=CIRCLE('',#10239,0.15);
#2495=CIRCLE('',#10240,0.15);
#2496=CIRCLE('',#10245,0.15);
#2497=CIRCLE('',#10246,0.15);
#2498=CIRCLE('',#10251,0.225);
#2499=CIRCLE('',#10252,0.225);
#2500=CIRCLE('',#10254,0.6);
#2501=CIRCLE('',#10255,0.6);
#2502=CIRCLE('',#10262,0.65);
#2503=CIRCLE('',#10263,0.65);
#2504=CIRCLE('',#10267,0.4);
#2505=CIRCLE('',#10268,0.4);
#2506=CIRCLE('',#10271,0.8);
#2507=CIRCLE('',#10272,0.0555);
#2508=CIRCLE('',#10273,0.611219772367581);
#2509=CIRCLE('',#10274,0.0555);
#2510=CIRCLE('',#10275,0.611219772367581);
#2511=CIRCLE('',#10276,0.0555);
#2512=CIRCLE('',#10277,0.611219772367581);
#2513=CIRCLE('',#10278,0.0555);
#2514=CIRCLE('',#10279,0.611219772367581);
#2515=CIRCLE('',#10280,0.0555);
#2516=CIRCLE('',#10281,0.611219772367581);
#2517=CIRCLE('',#10282,0.0555);
#2518=CIRCLE('',#10283,0.611219772367581);
#2519=CIRCLE('',#10284,0.0555);
#2520=CIRCLE('',#10285,0.611219772367581);
#2521=CIRCLE('',#10286,0.0555);
#2522=CIRCLE('',#10287,0.611219772367581);
#2523=CIRCLE('',#10288,0.0555);
#2524=CIRCLE('',#10289,0.611219772367581);
#2525=CIRCLE('',#10290,0.0555);
#2526=CIRCLE('',#10291,0.611219772367581);
#2527=CIRCLE('',#10292,0.0555);
#2528=CIRCLE('',#10293,0.611219772367581);
#2529=CIRCLE('',#10294,0.0555);
#2530=CIRCLE('',#10295,0.611219772367581);
#2531=CIRCLE('',#10296,0.0555);
#2532=CIRCLE('',#10297,0.611219772367581);
#2533=CIRCLE('',#10298,0.0555);
#2534=CIRCLE('',#10299,0.611219772367581);
#2535=CIRCLE('',#10300,0.0555);
#2536=CIRCLE('',#10301,0.611219772367581);
#2537=CIRCLE('',#10302,0.0555);
#2538=CIRCLE('',#10303,0.611219772367581);
#2539=CIRCLE('',#10304,0.0555);
#2540=CIRCLE('',#10305,0.611219772367581);
#2541=CIRCLE('',#10306,0.0555);
#2542=CIRCLE('',#10307,0.611219772367581);
#2543=CIRCLE('',#10308,0.0555);
#2544=CIRCLE('',#10309,0.611219772367581);
#2545=CIRCLE('',#10310,0.0555);
#2546=CIRCLE('',#10311,0.611219772367581);
#2547=CIRCLE('',#10313,0.8);
#2548=CIRCLE('',#10316,0.8);
#2549=CIRCLE('',#10317,0.0555);
#2550=CIRCLE('',#10318,0.611219772367581);
#2551=CIRCLE('',#10319,0.0555);
#2552=CIRCLE('',#10320,0.611219772367581);
#2553=CIRCLE('',#10321,0.0555);
#2554=CIRCLE('',#10322,0.611219772367581);
#2555=CIRCLE('',#10323,0.0555);
#2556=CIRCLE('',#10324,0.611219772367581);
#2557=CIRCLE('',#10325,0.0555);
#2558=CIRCLE('',#10326,0.611219772367581);
#2559=CIRCLE('',#10327,0.0555);
#2560=CIRCLE('',#10328,0.611219772367581);
#2561=CIRCLE('',#10329,0.0555);
#2562=CIRCLE('',#10330,0.611219772367581);
#2563=CIRCLE('',#10331,0.0555);
#2564=CIRCLE('',#10332,0.611219772367581);
#2565=CIRCLE('',#10333,0.0555);
#2566=CIRCLE('',#10334,0.611219772367581);
#2567=CIRCLE('',#10335,0.0555);
#2568=CIRCLE('',#10336,0.611219772367581);
#2569=CIRCLE('',#10337,0.0555);
#2570=CIRCLE('',#10338,0.611219772367581);
#2571=CIRCLE('',#10339,0.0555);
#2572=CIRCLE('',#10340,0.611219772367581);
#2573=CIRCLE('',#10341,0.0555);
#2574=CIRCLE('',#10342,0.611219772367581);
#2575=CIRCLE('',#10343,0.0555);
#2576=CIRCLE('',#10344,0.611219772367581);
#2577=CIRCLE('',#10345,0.0555);
#2578=CIRCLE('',#10346,0.611219772367581);
#2579=CIRCLE('',#10347,0.0555);
#2580=CIRCLE('',#10348,0.611219772367581);
#2581=CIRCLE('',#10349,0.0555);
#2582=CIRCLE('',#10350,0.611219772367581);
#2583=CIRCLE('',#10351,0.0555);
#2584=CIRCLE('',#10352,0.611219772367581);
#2585=CIRCLE('',#10353,0.0555);
#2586=CIRCLE('',#10354,0.611219772367581);
#2587=CIRCLE('',#10355,0.0555);
#2588=CIRCLE('',#10356,0.611219772367581);
#2589=CIRCLE('',#10358,0.8);
#2590=CIRCLE('',#10403,0.165);
#2591=CIRCLE('',#10404,0.165);
#2592=CIRCLE('',#10407,0.8);
#2593=CIRCLE('',#10408,0.6);
#2594=CIRCLE('',#10410,0.8);
#2595=CIRCLE('',#10411,0.6);
#2596=CIRCLE('',#10414,0.6);
#2597=CIRCLE('',#10417,0.6);
#2598=CIRCLE('',#10421,0.605);
#2599=CIRCLE('',#10422,0.605);
#2600=CIRCLE('',#10424,0.8);
#2601=CIRCLE('',#10425,0.8);
#2602=CIRCLE('',#10430,0.605);
#2603=CIRCLE('',#10431,0.605);
#2604=CIRCLE('',#10433,0.8);
#2605=CIRCLE('',#10434,0.8);
#2606=CIRCLE('',#10439,0.15);
#2607=CIRCLE('',#10440,0.15);
#2608=CIRCLE('',#10445,0.15);
#2609=CIRCLE('',#10446,0.15);
#2610=CIRCLE('',#10451,0.225);
#2611=CIRCLE('',#10452,0.225);
#2612=CIRCLE('',#10454,0.8);
#2613=CIRCLE('',#10455,0.8);
#2614=CIRCLE('',#10462,1.);
#2615=CIRCLE('',#10463,1.);
#2616=CIRCLE('',#10467,0.6);
#2617=CIRCLE('',#10468,0.6);
#2618=CIRCLE('',#10471,1.4);
#2619=CIRCLE('',#10472,0.0555000000000001);
#2620=CIRCLE('',#10473,1.24783954473516);
#2621=CIRCLE('',#10474,0.0555000000000001);
#2622=CIRCLE('',#10475,1.24783954473516);
#2623=CIRCLE('',#10476,0.0555000000000001);
#2624=CIRCLE('',#10477,1.24783954473516);
#2625=CIRCLE('',#10478,0.0555000000000001);
#2626=CIRCLE('',#10479,1.24783954473516);
#2627=CIRCLE('',#10480,0.0555000000000001);
#2628=CIRCLE('',#10481,1.24783954473516);
#2629=CIRCLE('',#10482,0.0555000000000001);
#2630=CIRCLE('',#10483,1.24783954473516);
#2631=CIRCLE('',#10484,0.0555000000000001);
#2632=CIRCLE('',#10485,1.24783954473516);
#2633=CIRCLE('',#10486,0.0555000000000001);
#2634=CIRCLE('',#10487,1.24783954473516);
#2635=CIRCLE('',#10488,0.0555000000000001);
#2636=CIRCLE('',#10489,1.24783954473516);
#2637=CIRCLE('',#10490,0.0555000000000001);
#2638=CIRCLE('',#10491,1.24783954473516);
#2639=CIRCLE('',#10492,0.0555000000000001);
#2640=CIRCLE('',#10493,1.24783954473516);
#2641=CIRCLE('',#10494,0.0555000000000001);
#2642=CIRCLE('',#10495,1.24783954473516);
#2643=CIRCLE('',#10496,0.0555000000000001);
#2644=CIRCLE('',#10497,1.24783954473516);
#2645=CIRCLE('',#10498,0.0555000000000001);
#2646=CIRCLE('',#10499,1.24783954473516);
#2647=CIRCLE('',#10500,0.0555000000000001);
#2648=CIRCLE('',#10501,1.24783954473516);
#2649=CIRCLE('',#10502,0.0555000000000001);
#2650=CIRCLE('',#10503,1.24783954473516);
#2651=CIRCLE('',#10504,0.0555000000000001);
#2652=CIRCLE('',#10505,1.24783954473516);
#2653=CIRCLE('',#10506,0.0555000000000001);
#2654=CIRCLE('',#10507,1.24783954473516);
#2655=CIRCLE('',#10508,0.0555000000000001);
#2656=CIRCLE('',#10509,1.24783954473516);
#2657=CIRCLE('',#10510,0.0555000000000001);
#2658=CIRCLE('',#10511,1.24783954473516);
#2659=CIRCLE('',#10512,0.0555000000000001);
#2660=CIRCLE('',#10513,1.24783954473516);
#2661=CIRCLE('',#10514,0.0555000000000001);
#2662=CIRCLE('',#10515,1.24783954473516);
#2663=CIRCLE('',#10516,0.0555000000000001);
#2664=CIRCLE('',#10517,1.24783954473516);
#2665=CIRCLE('',#10518,0.0555000000000001);
#2666=CIRCLE('',#10519,1.24783954473516);
#2667=CIRCLE('',#10520,0.0555000000000001);
#2668=CIRCLE('',#10521,1.24783954473516);
#2669=CIRCLE('',#10522,0.0555000000000001);
#2670=CIRCLE('',#10523,1.24783954473516);
#2671=CIRCLE('',#10524,0.0555000000000001);
#2672=CIRCLE('',#10525,1.24783954473516);
#2673=CIRCLE('',#10526,0.0555000000000001);
#2674=CIRCLE('',#10527,1.24783954473516);
#2675=CIRCLE('',#10528,0.0555000000000001);
#2676=CIRCLE('',#10529,1.24783954473516);
#2677=CIRCLE('',#10530,0.0555000000000001);
#2678=CIRCLE('',#10531,1.24783954473516);
#2679=CIRCLE('',#10532,0.0555000000000001);
#2680=CIRCLE('',#10533,1.24783954473516);
#2681=CIRCLE('',#10534,0.0555000000000001);
#2682=CIRCLE('',#10535,1.24783954473516);
#2683=CIRCLE('',#10536,0.0555000000000001);
#2684=CIRCLE('',#10537,1.24783954473516);
#2685=CIRCLE('',#10538,0.0555000000000001);
#2686=CIRCLE('',#10539,1.24783954473516);
#2687=CIRCLE('',#10540,0.0555000000000001);
#2688=CIRCLE('',#10541,1.24783954473516);
#2689=CIRCLE('',#10542,0.0555000000000001);
#2690=CIRCLE('',#10543,1.24783954473516);
#2691=CIRCLE('',#10544,0.0555000000000001);
#2692=CIRCLE('',#10545,1.24783954473516);
#2693=CIRCLE('',#10546,0.0555000000000001);
#2694=CIRCLE('',#10547,1.24783954473516);
#2695=CIRCLE('',#10548,0.0555000000000001);
#2696=CIRCLE('',#10549,1.24783954473516);
#2697=CIRCLE('',#10550,0.0555000000000001);
#2698=CIRCLE('',#10551,1.24783954473516);
#2699=CIRCLE('',#10553,1.4);
#2700=CIRCLE('',#10556,1.4);
#2701=CIRCLE('',#10557,0.0555000000000001);
#2702=CIRCLE('',#10558,1.24783954473516);
#2703=CIRCLE('',#10559,0.0555000000000001);
#2704=CIRCLE('',#10560,1.24783954473516);
#2705=CIRCLE('',#10561,0.0555000000000001);
#2706=CIRCLE('',#10562,1.24783954473516);
#2707=CIRCLE('',#10563,0.0555000000000001);
#2708=CIRCLE('',#10564,1.24783954473516);
#2709=CIRCLE('',#10565,0.0555000000000001);
#2710=CIRCLE('',#10566,1.24783954473516);
#2711=CIRCLE('',#10567,0.0555000000000001);
#2712=CIRCLE('',#10568,1.24783954473516);
#2713=CIRCLE('',#10569,0.0555000000000001);
#2714=CIRCLE('',#10570,1.24783954473516);
#2715=CIRCLE('',#10571,0.0555000000000001);
#2716=CIRCLE('',#10572,1.24783954473516);
#2717=CIRCLE('',#10573,0.0555000000000001);
#2718=CIRCLE('',#10574,1.24783954473516);
#2719=CIRCLE('',#10575,0.0555000000000001);
#2720=CIRCLE('',#10576,1.24783954473516);
#2721=CIRCLE('',#10577,0.0555000000000001);
#2722=CIRCLE('',#10578,1.24783954473516);
#2723=CIRCLE('',#10579,0.0555000000000001);
#2724=CIRCLE('',#10580,1.24783954473516);
#2725=CIRCLE('',#10581,0.0555000000000001);
#2726=CIRCLE('',#10582,1.24783954473516);
#2727=CIRCLE('',#10583,0.0555000000000001);
#2728=CIRCLE('',#10584,1.24783954473516);
#2729=CIRCLE('',#10585,0.0555000000000001);
#2730=CIRCLE('',#10586,1.24783954473516);
#2731=CIRCLE('',#10587,0.0555000000000001);
#2732=CIRCLE('',#10588,1.24783954473516);
#2733=CIRCLE('',#10589,0.0555000000000001);
#2734=CIRCLE('',#10590,1.24783954473516);
#2735=CIRCLE('',#10591,0.0555000000000001);
#2736=CIRCLE('',#10592,1.24783954473516);
#2737=CIRCLE('',#10593,0.0555000000000001);
#2738=CIRCLE('',#10594,1.24783954473516);
#2739=CIRCLE('',#10595,0.0555000000000001);
#2740=CIRCLE('',#10596,1.24783954473516);
#2741=CIRCLE('',#10597,0.0555000000000001);
#2742=CIRCLE('',#10598,1.24783954473516);
#2743=CIRCLE('',#10599,0.0555000000000001);
#2744=CIRCLE('',#10600,1.24783954473516);
#2745=CIRCLE('',#10601,0.0555000000000001);
#2746=CIRCLE('',#10602,1.24783954473516);
#2747=CIRCLE('',#10603,0.0555000000000001);
#2748=CIRCLE('',#10604,1.24783954473516);
#2749=CIRCLE('',#10605,0.0555000000000001);
#2750=CIRCLE('',#10606,1.24783954473516);
#2751=CIRCLE('',#10607,0.0555000000000001);
#2752=CIRCLE('',#10608,1.24783954473516);
#2753=CIRCLE('',#10609,0.0555000000000001);
#2754=CIRCLE('',#10610,1.24783954473516);
#2755=CIRCLE('',#10611,0.0555000000000001);
#2756=CIRCLE('',#10612,1.24783954473516);
#2757=CIRCLE('',#10613,0.0555000000000001);
#2758=CIRCLE('',#10614,1.24783954473516);
#2759=CIRCLE('',#10615,0.0555000000000001);
#2760=CIRCLE('',#10616,1.24783954473516);
#2761=CIRCLE('',#10617,0.0555000000000001);
#2762=CIRCLE('',#10618,1.24783954473516);
#2763=CIRCLE('',#10619,0.0555000000000001);
#2764=CIRCLE('',#10620,1.24783954473516);
#2765=CIRCLE('',#10621,0.0555000000000001);
#2766=CIRCLE('',#10622,1.24783954473516);
#2767=CIRCLE('',#10623,0.0555000000000001);
#2768=CIRCLE('',#10624,1.24783954473516);
#2769=CIRCLE('',#10625,0.0555000000000001);
#2770=CIRCLE('',#10626,1.24783954473516);
#2771=CIRCLE('',#10627,0.0555000000000001);
#2772=CIRCLE('',#10628,1.24783954473516);
#2773=CIRCLE('',#10629,0.0555000000000001);
#2774=CIRCLE('',#10630,1.24783954473516);
#2775=CIRCLE('',#10631,0.0555000000000001);
#2776=CIRCLE('',#10632,1.24783954473516);
#2777=CIRCLE('',#10633,0.0555000000000001);
#2778=CIRCLE('',#10634,1.24783954473516);
#2779=CIRCLE('',#10635,0.0555000000000001);
#2780=CIRCLE('',#10636,1.24783954473516);
#2781=CIRCLE('',#10638,1.4);
#2782=CIRCLE('',#10722,0.3);
#2783=CIRCLE('',#10724,0.35);
#2784=CIRCLE('',#10726,0.35);
#2785=CIRCLE('',#10728,0.32);
#2786=CIRCLE('',#10730,0.22);
#2787=CIRCLE('',#10732,0.1954);
#2788=CIRCLE('',#10734,0.1954);
#2789=CIRCLE('',#10736,0.16);
#2790=LINE('',#13879,#3268);
#2791=LINE('',#13883,#3269);
#2792=LINE('',#13888,#3270);
#2793=LINE('',#13892,#3271);
#2794=LINE('',#13897,#3272);
#2795=LINE('',#13899,#3273);
#2796=LINE('',#13901,#3274);
#2797=LINE('',#13902,#3275);
#2798=LINE('',#13907,#3276);
#2799=LINE('',#13910,#3277);
#2800=LINE('',#13915,#3278);
#2801=LINE('',#13918,#3279);
#2802=LINE('',#13923,#3280);
#2803=LINE('',#13926,#3281);
#2804=LINE('',#13927,#3282);
#2805=LINE('',#13928,#3283);
#2806=LINE('',#13930,#3284);
#2807=LINE('',#13932,#3285);
#2808=LINE('',#13935,#3286);
#2809=LINE('',#13937,#3287);
#2810=LINE('',#13941,#3288);
#2811=LINE('',#13944,#3289);
#2812=LINE('',#13946,#3290);
#2813=LINE('',#13948,#3291);
#2814=LINE('',#13952,#3292);
#2815=LINE('',#13955,#3293);
#2816=LINE('',#13957,#3294);
#2817=LINE('',#13961,#3295);
#2818=LINE('',#13965,#3296);
#2819=LINE('',#13968,#3297);
#2820=LINE('',#13970,#3298);
#2821=LINE('',#13972,#3299);
#2822=LINE('',#13976,#3300);
#2823=LINE('',#13979,#3301);
#2824=LINE('',#13981,#3302);
#2825=LINE('',#13985,#3303);
#2826=LINE('',#13989,#3304);
#2827=LINE('',#13992,#3305);
#2828=LINE('',#13994,#3306);
#2829=LINE('',#13996,#3307);
#2830=LINE('',#14005,#3308);
#2831=LINE('',#14012,#3309);
#2832=LINE('',#14021,#3310);
#2833=LINE('',#14023,#3311);
#2834=LINE('',#14024,#3312);
#2835=LINE('',#14027,#3313);
#2836=LINE('',#14028,#3314);
#2837=LINE('',#14031,#3315);
#2838=LINE('',#14032,#3316);
#2839=LINE('',#14034,#3317);
#2840=LINE('',#14040,#3318);
#2841=LINE('',#14042,#3319);
#2842=LINE('',#14044,#3320);
#2843=LINE('',#14045,#3321);
#2844=LINE('',#14048,#3322);
#2845=LINE('',#14050,#3323);
#2846=LINE('',#14051,#3324);
#2847=LINE('',#14054,#3325);
#2848=LINE('',#14056,#3326);
#2849=LINE('',#14057,#3327);
#2850=LINE('',#14059,#3328);
#2851=LINE('',#14060,#3329);
#2852=LINE('',#14067,#3330);
#2853=LINE('',#14069,#3331);
#2854=LINE('',#14071,#3332);
#2855=LINE('',#14072,#3333);
#2856=LINE('',#14075,#3334);
#2857=LINE('',#14077,#3335);
#2858=LINE('',#14078,#3336);
#2859=LINE('',#14081,#3337);
#2860=LINE('',#14083,#3338);
#2861=LINE('',#14084,#3339);
#2862=LINE('',#14086,#3340);
#2863=LINE('',#14087,#3341);
#2864=LINE('',#14095,#3342);
#2865=LINE('',#14101,#3343);
#2866=LINE('',#14107,#3344);
#2867=LINE('',#14113,#3345);
#2868=LINE('',#14119,#3346);
#2869=LINE('',#14125,#3347);
#2870=LINE('',#14131,#3348);
#2871=LINE('',#14137,#3349);
#2872=LINE('',#14143,#3350);
#2873=LINE('',#14148,#3351);
#2874=LINE('',#14150,#3352);
#2875=LINE('',#14152,#3353);
#2876=LINE('',#14153,#3354);
#2877=LINE('',#14157,#3355);
#2878=LINE('',#14159,#3356);
#2879=LINE('',#14161,#3357);
#2880=LINE('',#14162,#3358);
#2881=LINE('',#14165,#3359);
#2882=LINE('',#14167,#3360);
#2883=LINE('',#14168,#3361);
#2884=LINE('',#14171,#3362);
#2885=LINE('',#14173,#3363);
#2886=LINE('',#14174,#3364);
#2887=LINE('',#14177,#3365);
#2888=LINE('',#14179,#3366);
#2889=LINE('',#14180,#3367);
#2890=LINE('',#14181,#3368);
#2891=LINE('',#14184,#3369);
#2892=LINE('',#14185,#3370);
#2893=LINE('',#14188,#3371);
#2894=LINE('',#14189,#3372);
#2895=LINE('',#14190,#3373);
#2896=LINE('',#14192,#3374);
#2897=LINE('',#14200,#3375);
#2898=LINE('',#14206,#3376);
#2899=LINE('',#14214,#3377);
#2900=LINE('',#14218,#3378);
#2901=LINE('',#14223,#3379);
#2902=LINE('',#14227,#3380);
#2903=LINE('',#14232,#3381);
#2904=LINE('',#14236,#3382);
#2905=LINE('',#14241,#3383);
#2906=LINE('',#14245,#3384);
#2907=LINE('',#14266,#3385);
#2908=LINE('',#14272,#3386);
#2909=LINE('',#14278,#3387);
#2910=LINE('',#14282,#3388);
#2911=LINE('',#14287,#3389);
#2912=LINE('',#14291,#3390);
#2913=LINE('',#14296,#3391);
#2914=LINE('',#14300,#3392);
#2915=LINE('',#14305,#3393);
#2916=LINE('',#14309,#3394);
#2917=LINE('',#14328,#3395);
#2918=LINE('',#14336,#3396);
#2919=LINE('',#14343,#3397);
#2920=LINE('',#14349,#3398);
#2921=LINE('',#14355,#3399);
#2922=LINE('',#14361,#3400);
#2923=LINE('',#14367,#3401);
#2924=LINE('',#14373,#3402);
#2925=LINE('',#14379,#3403);
#2926=LINE('',#14385,#3404);
#2927=LINE('',#14391,#3405);
#2928=LINE('',#14396,#3406);
#2929=LINE('',#14398,#3407);
#2930=LINE('',#14400,#3408);
#2931=LINE('',#14401,#3409);
#2932=LINE('',#14405,#3410);
#2933=LINE('',#14407,#3411);
#2934=LINE('',#14409,#3412);
#2935=LINE('',#14410,#3413);
#2936=LINE('',#14413,#3414);
#2937=LINE('',#14415,#3415);
#2938=LINE('',#14416,#3416);
#2939=LINE('',#14419,#3417);
#2940=LINE('',#14421,#3418);
#2941=LINE('',#14422,#3419);
#2942=LINE('',#14425,#3420);
#2943=LINE('',#14427,#3421);
#2944=LINE('',#14428,#3422);
#2945=LINE('',#14429,#3423);
#2946=LINE('',#14432,#3424);
#2947=LINE('',#14433,#3425);
#2948=LINE('',#14436,#3426);
#2949=LINE('',#14437,#3427);
#2950=LINE('',#14438,#3428);
#2951=LINE('',#14440,#3429);
#2952=LINE('',#14448,#3430);
#2953=LINE('',#14454,#3431);
#2954=LINE('',#14463,#3432);
#2955=LINE('',#14469,#3433);
#2956=LINE('',#14478,#3434);
#2957=LINE('',#14484,#3435);
#2958=LINE('',#14493,#3436);
#2959=LINE('',#14499,#3437);
#2960=LINE('',#14508,#3438);
#2961=LINE('',#14514,#3439);
#2962=LINE('',#14522,#3440);
#2963=LINE('',#14526,#3441);
#2964=LINE('',#14531,#3442);
#2965=LINE('',#14535,#3443);
#2966=LINE('',#14540,#3444);
#2967=LINE('',#14544,#3445);
#2968=LINE('',#14549,#3446);
#2969=LINE('',#14553,#3447);
#2970=LINE('',#14574,#3448);
#2971=LINE('',#14580,#3449);
#2972=LINE('',#14586,#3450);
#2973=LINE('',#14590,#3451);
#2974=LINE('',#14595,#3452);
#2975=LINE('',#14599,#3453);
#2976=LINE('',#14604,#3454);
#2977=LINE('',#14608,#3455);
#2978=LINE('',#14613,#3456);
#2979=LINE('',#14617,#3457);
#2980=LINE('',#14636,#3458);
#2981=LINE('',#14644,#3459);
#2982=LINE('',#14650,#3460);
#2983=LINE('',#14652,#3461);
#2984=LINE('',#14654,#3462);
#2985=LINE('',#14655,#3463);
#2986=LINE('',#14659,#3464);
#2987=LINE('',#14661,#3465);
#2988=LINE('',#14663,#3466);
#2989=LINE('',#14664,#3467);
#2990=LINE('',#14668,#3468);
#2991=LINE('',#14672,#3469);
#2992=LINE('',#14682,#3470);
#2993=LINE('',#14685,#3471);
#2994=LINE('',#14688,#3472);
#2995=LINE('',#14689,#3473);
#2996=LINE('',#14692,#3474);
#2997=LINE('',#14693,#3475);
#2998=LINE('',#14711,#3476);
#2999=LINE('',#14717,#3477);
#3000=LINE('',#14721,#3478);
#3001=LINE('',#14727,#3479);
#3002=LINE('',#14732,#3480);
#3003=LINE('',#14747,#3481);
#3004=LINE('',#14756,#3482);
#3005=LINE('',#14760,#3483);
#3006=LINE('',#14764,#3484);
#3007=LINE('',#14767,#3485);
#3008=LINE('',#14920,#3486);
#3009=LINE('',#15216,#3487);
#3010=LINE('',#15258,#3488);
#3011=LINE('',#15263,#3489);
#3012=LINE('',#15272,#3490);
#3013=LINE('',#15277,#3491);
#3014=LINE('',#15287,#3492);
#3015=LINE('',#15289,#3493);
#3016=LINE('',#15291,#3494);
#3017=LINE('',#15292,#3495);
#3018=LINE('',#15295,#3496);
#3019=LINE('',#15297,#3497);
#3020=LINE('',#15298,#3498);
#3021=LINE('',#15301,#3499);
#3022=LINE('',#15303,#3500);
#3023=LINE('',#15304,#3501);
#3024=LINE('',#15307,#3502);
#3025=LINE('',#15309,#3503);
#3026=LINE('',#15310,#3504);
#3027=LINE('',#15313,#3505);
#3028=LINE('',#15315,#3506);
#3029=LINE('',#15316,#3507);
#3030=LINE('',#15318,#3508);
#3031=LINE('',#15319,#3509);
#3032=LINE('',#15329,#3510);
#3033=LINE('',#15338,#3511);
#3034=LINE('',#15342,#3512);
#3035=LINE('',#15346,#3513);
#3036=LINE('',#15353,#3514);
#3037=LINE('',#15357,#3515);
#3038=LINE('',#15359,#3516);
#3039=LINE('',#15374,#3517);
#3040=LINE('',#15380,#3518);
#3041=LINE('',#15384,#3519);
#3042=LINE('',#15390,#3520);
#3043=LINE('',#15395,#3521);
#3044=LINE('',#15410,#3522);
#3045=LINE('',#15419,#3523);
#3046=LINE('',#15423,#3524);
#3047=LINE('',#15427,#3525);
#3048=LINE('',#15430,#3526);
#3049=LINE('',#15566,#3527);
#3050=LINE('',#15819,#3528);
#3051=LINE('',#15861,#3529);
#3052=LINE('',#15866,#3530);
#3053=LINE('',#15875,#3531);
#3054=LINE('',#15880,#3532);
#3055=LINE('',#15890,#3533);
#3056=LINE('',#15892,#3534);
#3057=LINE('',#15894,#3535);
#3058=LINE('',#15895,#3536);
#3059=LINE('',#15898,#3537);
#3060=LINE('',#15900,#3538);
#3061=LINE('',#15901,#3539);
#3062=LINE('',#15904,#3540);
#3063=LINE('',#15906,#3541);
#3064=LINE('',#15907,#3542);
#3065=LINE('',#15910,#3543);
#3066=LINE('',#15912,#3544);
#3067=LINE('',#15913,#3545);
#3068=LINE('',#15916,#3546);
#3069=LINE('',#15918,#3547);
#3070=LINE('',#15919,#3548);
#3071=LINE('',#15921,#3549);
#3072=LINE('',#15922,#3550);
#3073=LINE('',#15934,#3551);
#3074=LINE('',#15938,#3552);
#3075=LINE('',#15942,#3553);
#3076=LINE('',#15949,#3554);
#3077=LINE('',#15951,#3555);
#3078=LINE('',#15958,#3556);
#3079=LINE('',#15972,#3557);
#3080=LINE('',#15975,#3558);
#3081=LINE('',#15981,#3559);
#3082=LINE('',#15987,#3560);
#3083=LINE('',#15995,#3561);
#3084=LINE('',#16002,#3562);
#3085=LINE('',#16008,#3563);
#3086=LINE('',#16017,#3564);
#3087=LINE('',#16023,#3565);
#3088=LINE('',#16032,#3566);
#3089=LINE('',#16041,#3567);
#3090=LINE('',#16050,#3568);
#3091=LINE('',#16056,#3569);
#3092=LINE('',#16104,#3570);
#3093=LINE('',#16188,#3571);
#3094=LINE('',#16232,#3572);
#3095=LINE('',#16234,#3573);
#3096=LINE('',#16320,#3574);
#3097=LINE('',#16397,#3575);
#3098=LINE('',#16401,#3576);
#3099=LINE('',#16403,#3577);
#3100=LINE('',#16492,#3578);
#3101=LINE('',#16580,#3579);
#3102=LINE('',#16583,#3580);
#3103=LINE('',#16584,#3581);
#3104=LINE('',#16586,#3582);
#3105=LINE('',#16588,#3583);
#3106=LINE('',#16590,#3584);
#3107=LINE('',#16592,#3585);
#3108=LINE('',#16594,#3586);
#3109=LINE('',#16596,#3587);
#3110=LINE('',#16598,#3588);
#3111=LINE('',#16600,#3589);
#3112=LINE('',#16602,#3590);
#3113=LINE('',#16604,#3591);
#3114=LINE('',#16606,#3592);
#3115=LINE('',#16608,#3593);
#3116=LINE('',#16610,#3594);
#3117=LINE('',#16612,#3595);
#3118=LINE('',#16614,#3596);
#3119=LINE('',#16616,#3597);
#3120=LINE('',#16618,#3598);
#3121=LINE('',#16620,#3599);
#3122=LINE('',#16622,#3600);
#3123=LINE('',#16624,#3601);
#3124=LINE('',#16626,#3602);
#3125=LINE('',#16628,#3603);
#3126=LINE('',#16630,#3604);
#3127=LINE('',#16632,#3605);
#3128=LINE('',#16634,#3606);
#3129=LINE('',#16636,#3607);
#3130=LINE('',#16638,#3608);
#3131=LINE('',#16640,#3609);
#3132=LINE('',#16642,#3610);
#3133=LINE('',#16644,#3611);
#3134=LINE('',#16646,#3612);
#3135=LINE('',#16648,#3613);
#3136=LINE('',#16650,#3614);
#3137=LINE('',#16652,#3615);
#3138=LINE('',#16654,#3616);
#3139=LINE('',#16656,#3617);
#3140=LINE('',#16658,#3618);
#3141=LINE('',#16660,#3619);
#3142=LINE('',#16668,#3620);
#3143=LINE('',#16682,#3621);
#3144=LINE('',#16685,#3622);
#3145=LINE('',#16691,#3623);
#3146=LINE('',#16698,#3624);
#3147=LINE('',#16704,#3625);
#3148=LINE('',#16713,#3626);
#3149=LINE('',#16719,#3627);
#3150=LINE('',#16728,#3628);
#3151=LINE('',#16737,#3629);
#3152=LINE('',#16746,#3630);
#3153=LINE('',#16752,#3631);
#3154=LINE('',#16800,#3632);
#3155=LINE('',#16884,#3633);
#3156=LINE('',#16928,#3634);
#3157=LINE('',#16930,#3635);
#3158=LINE('',#17016,#3636);
#3159=LINE('',#17093,#3637);
#3160=LINE('',#17097,#3638);
#3161=LINE('',#17099,#3639);
#3162=LINE('',#17268,#3640);
#3163=LINE('',#17436,#3641);
#3164=LINE('',#17439,#3642);
#3165=LINE('',#17440,#3643);
#3166=LINE('',#17442,#3644);
#3167=LINE('',#17444,#3645);
#3168=LINE('',#17446,#3646);
#3169=LINE('',#17448,#3647);
#3170=LINE('',#17450,#3648);
#3171=LINE('',#17452,#3649);
#3172=LINE('',#17454,#3650);
#3173=LINE('',#17456,#3651);
#3174=LINE('',#17458,#3652);
#3175=LINE('',#17460,#3653);
#3176=LINE('',#17462,#3654);
#3177=LINE('',#17464,#3655);
#3178=LINE('',#17466,#3656);
#3179=LINE('',#17468,#3657);
#3180=LINE('',#17470,#3658);
#3181=LINE('',#17472,#3659);
#3182=LINE('',#17474,#3660);
#3183=LINE('',#17476,#3661);
#3184=LINE('',#17478,#3662);
#3185=LINE('',#17480,#3663);
#3186=LINE('',#17482,#3664);
#3187=LINE('',#17484,#3665);
#3188=LINE('',#17486,#3666);
#3189=LINE('',#17488,#3667);
#3190=LINE('',#17490,#3668);
#3191=LINE('',#17492,#3669);
#3192=LINE('',#17494,#3670);
#3193=LINE('',#17496,#3671);
#3194=LINE('',#17498,#3672);
#3195=LINE('',#17500,#3673);
#3196=LINE('',#17502,#3674);
#3197=LINE('',#17504,#3675);
#3198=LINE('',#17506,#3676);
#3199=LINE('',#17508,#3677);
#3200=LINE('',#17510,#3678);
#3201=LINE('',#17512,#3679);
#3202=LINE('',#17514,#3680);
#3203=LINE('',#17516,#3681);
#3204=LINE('',#17518,#3682);
#3205=LINE('',#17520,#3683);
#3206=LINE('',#17522,#3684);
#3207=LINE('',#17524,#3685);
#3208=LINE('',#17526,#3686);
#3209=LINE('',#17528,#3687);
#3210=LINE('',#17530,#3688);
#3211=LINE('',#17532,#3689);
#3212=LINE('',#17534,#3690);
#3213=LINE('',#17536,#3691);
#3214=LINE('',#17538,#3692);
#3215=LINE('',#17540,#3693);
#3216=LINE('',#17542,#3694);
#3217=LINE('',#17544,#3695);
#3218=LINE('',#17546,#3696);
#3219=LINE('',#17548,#3697);
#3220=LINE('',#17550,#3698);
#3221=LINE('',#17552,#3699);
#3222=LINE('',#17554,#3700);
#3223=LINE('',#17556,#3701);
#3224=LINE('',#17558,#3702);
#3225=LINE('',#17560,#3703);
#3226=LINE('',#17562,#3704);
#3227=LINE('',#17564,#3705);
#3228=LINE('',#17566,#3706);
#3229=LINE('',#17568,#3707);
#3230=LINE('',#17570,#3708);
#3231=LINE('',#17572,#3709);
#3232=LINE('',#17574,#3710);
#3233=LINE('',#17576,#3711);
#3234=LINE('',#17578,#3712);
#3235=LINE('',#17580,#3713);
#3236=LINE('',#17582,#3714);
#3237=LINE('',#17584,#3715);
#3238=LINE('',#17586,#3716);
#3239=LINE('',#17588,#3717);
#3240=LINE('',#17590,#3718);
#3241=LINE('',#17592,#3719);
#3242=LINE('',#17594,#3720);
#3243=LINE('',#17596,#3721);
#3244=LINE('',#17605,#3722);
#3245=LINE('',#17609,#3723);
#3246=LINE('',#17613,#3724);
#3247=LINE('',#17620,#3725);
#3248=LINE('',#17624,#3726);
#3249=LINE('',#17628,#3727);
#3250=LINE('',#17633,#3728);
#3251=LINE('',#17635,#3729);
#3252=LINE('',#17637,#3730);
#3253=LINE('',#17638,#3731);
#3254=LINE('',#17641,#3732);
#3255=LINE('',#17643,#3733);
#3256=LINE('',#17644,#3734);
#3257=LINE('',#17647,#3735);
#3258=LINE('',#17649,#3736);
#3259=LINE('',#17650,#3737);
#3260=LINE('',#17653,#3738);
#3261=LINE('',#17655,#3739);
#3262=LINE('',#17656,#3740);
#3263=LINE('',#17659,#3741);
#3264=LINE('',#17661,#3742);
#3265=LINE('',#17662,#3743);
#3266=LINE('',#17664,#3744);
#3267=LINE('',#17665,#3745);
#3268=VECTOR('',#10817,1.);
#3269=VECTOR('',#10820,1.);
#3270=VECTOR('',#10825,1.);
#3271=VECTOR('',#10828,1.);
#3272=VECTOR('',#10833,1.);
#3273=VECTOR('',#10834,1.);
#3274=VECTOR('',#10835,1.);
#3275=VECTOR('',#10836,1.);
#3276=VECTOR('',#10839,1.);
#3277=VECTOR('',#10842,1.);
#3278=VECTOR('',#10845,1.);
#3279=VECTOR('',#10848,1.);
#3280=VECTOR('',#10851,1.);
#3281=VECTOR('',#10854,1.);
#3282=VECTOR('',#10855,1.);
#3283=VECTOR('',#10856,1.);
#3284=VECTOR('',#10859,1.);
#3285=VECTOR('',#10862,1.);
#3286=VECTOR('',#10865,1.);
#3287=VECTOR('',#10866,1.);
#3288=VECTOR('',#10871,1.);
#3289=VECTOR('',#10874,1.);
#3290=VECTOR('',#10877,1.);
#3291=VECTOR('',#10880,1.);
#3292=VECTOR('',#10883,1.);
#3293=VECTOR('',#10886,1.);
#3294=VECTOR('',#10887,1.);
#3295=VECTOR('',#10890,1.);
#3296=VECTOR('',#10895,1.);
#3297=VECTOR('',#10898,1.);
#3298=VECTOR('',#10901,1.);
#3299=VECTOR('',#10904,1.);
#3300=VECTOR('',#10907,1.);
#3301=VECTOR('',#10910,1.);
#3302=VECTOR('',#10911,1.);
#3303=VECTOR('',#10914,1.);
#3304=VECTOR('',#10919,1.);
#3305=VECTOR('',#10922,1.);
#3306=VECTOR('',#10925,1.);
#3307=VECTOR('',#10928,1.);
#3308=VECTOR('',#10941,0.165);
#3309=VECTOR('',#10950,0.165);
#3310=VECTOR('',#10965,1.);
#3311=VECTOR('',#10966,1.);
#3312=VECTOR('',#10967,1.);
#3313=VECTOR('',#10970,1.);
#3314=VECTOR('',#10971,1.);
#3315=VECTOR('',#10974,1.);
#3316=VECTOR('',#10975,1.);
#3317=VECTOR('',#10978,1.);
#3318=VECTOR('',#10985,1.);
#3319=VECTOR('',#10986,1.);
#3320=VECTOR('',#10987,1.);
#3321=VECTOR('',#10988,1.);
#3322=VECTOR('',#10991,1.);
#3323=VECTOR('',#10992,1.);
#3324=VECTOR('',#10993,1.);
#3325=VECTOR('',#10996,1.);
#3326=VECTOR('',#10997,1.);
#3327=VECTOR('',#10998,1.);
#3328=VECTOR('',#11001,1.);
#3329=VECTOR('',#11002,1.);
#3330=VECTOR('',#11011,1.);
#3331=VECTOR('',#11012,1.);
#3332=VECTOR('',#11013,1.);
#3333=VECTOR('',#11014,1.);
#3334=VECTOR('',#11017,1.);
#3335=VECTOR('',#11018,1.);
#3336=VECTOR('',#11019,1.);
#3337=VECTOR('',#11022,1.);
#3338=VECTOR('',#11023,1.);
#3339=VECTOR('',#11024,1.);
#3340=VECTOR('',#11027,1.);
#3341=VECTOR('',#11028,1.);
#3342=VECTOR('',#11039,0.165);
#3343=VECTOR('',#11046,0.165);
#3344=VECTOR('',#11053,0.165);
#3345=VECTOR('',#11060,0.165);
#3346=VECTOR('',#11067,1.5);
#3347=VECTOR('',#11074,0.225);
#3348=VECTOR('',#11081,0.225);
#3349=VECTOR('',#11088,0.225);
#3350=VECTOR('',#11095,0.225);
#3351=VECTOR('',#11100,1.);
#3352=VECTOR('',#11101,1.);
#3353=VECTOR('',#11102,1.);
#3354=VECTOR('',#11103,1.);
#3355=VECTOR('',#11106,1.);
#3356=VECTOR('',#11107,1.);
#3357=VECTOR('',#11108,1.);
#3358=VECTOR('',#11109,1.);
#3359=VECTOR('',#11112,1.);
#3360=VECTOR('',#11113,1.);
#3361=VECTOR('',#11114,1.);
#3362=VECTOR('',#11117,1.);
#3363=VECTOR('',#11118,1.);
#3364=VECTOR('',#11119,1.);
#3365=VECTOR('',#11122,1.);
#3366=VECTOR('',#11123,1.);
#3367=VECTOR('',#11124,1.);
#3368=VECTOR('',#11125,1.);
#3369=VECTOR('',#11128,1.);
#3370=VECTOR('',#11129,1.);
#3371=VECTOR('',#11132,1.);
#3372=VECTOR('',#11133,1.);
#3373=VECTOR('',#11134,1.);
#3374=VECTOR('',#11137,1.);
#3375=VECTOR('',#11148,1.1);
#3376=VECTOR('',#11155,1.49);
#3377=VECTOR('',#11166,1.);
#3378=VECTOR('',#11169,1.);
#3379=VECTOR('',#11174,1.);
#3380=VECTOR('',#11177,1.);
#3381=VECTOR('',#11182,1.);
#3382=VECTOR('',#11185,1.);
#3383=VECTOR('',#11190,1.);
#3384=VECTOR('',#11193,1.);
#3385=VECTOR('',#11228,1.49);
#3386=VECTOR('',#11237,1.1);
#3387=VECTOR('',#11244,1.);
#3388=VECTOR('',#11247,1.);
#3389=VECTOR('',#11252,1.);
#3390=VECTOR('',#11255,1.);
#3391=VECTOR('',#11260,1.);
#3392=VECTOR('',#11263,1.);
#3393=VECTOR('',#11268,1.);
#3394=VECTOR('',#11271,1.);
#3395=VECTOR('',#11304,1.49);
#3396=VECTOR('',#11315,1.1);
#3397=VECTOR('',#11324,0.165);
#3398=VECTOR('',#11331,0.165);
#3399=VECTOR('',#11338,0.164999999999999);
#3400=VECTOR('',#11345,0.164999999999999);
#3401=VECTOR('',#11352,1.6);
#3402=VECTOR('',#11359,0.225);
#3403=VECTOR('',#11366,0.225);
#3404=VECTOR('',#11373,0.225);
#3405=VECTOR('',#11380,0.225);
#3406=VECTOR('',#11385,1.);
#3407=VECTOR('',#11386,1.);
#3408=VECTOR('',#11387,1.);
#3409=VECTOR('',#11388,1.);
#3410=VECTOR('',#11391,1.);
#3411=VECTOR('',#11392,1.);
#3412=VECTOR('',#11393,1.);
#3413=VECTOR('',#11394,1.);
#3414=VECTOR('',#11397,1.);
#3415=VECTOR('',#11398,1.);
#3416=VECTOR('',#11399,1.);
#3417=VECTOR('',#11402,1.);
#3418=VECTOR('',#11403,1.);
#3419=VECTOR('',#11404,1.);
#3420=VECTOR('',#11407,1.);
#3421=VECTOR('',#11408,1.);
#3422=VECTOR('',#11409,1.);
#3423=VECTOR('',#11410,1.);
#3424=VECTOR('',#11413,1.);
#3425=VECTOR('',#11414,1.);
#3426=VECTOR('',#11417,1.);
#3427=VECTOR('',#11418,1.);
#3428=VECTOR('',#11419,1.);
#3429=VECTOR('',#11422,1.);
#3430=VECTOR('',#11433,0.165);
#3431=VECTOR('',#11440,0.4);
#3432=VECTOR('',#11453,0.165);
#3433=VECTOR('',#11460,0.4);
#3434=VECTOR('',#11473,0.164999999999999);
#3435=VECTOR('',#11480,0.4);
#3436=VECTOR('',#11493,0.164999999999999);
#3437=VECTOR('',#11500,0.4);
#3438=VECTOR('',#11513,1.2);
#3439=VECTOR('',#11520,1.59);
#3440=VECTOR('',#11531,1.);
#3441=VECTOR('',#11534,1.);
#3442=VECTOR('',#11539,1.);
#3443=VECTOR('',#11542,1.);
#3444=VECTOR('',#11547,1.);
#3445=VECTOR('',#11550,1.);
#3446=VECTOR('',#11555,1.);
#3447=VECTOR('',#11558,1.);
#3448=VECTOR('',#11593,1.59);
#3449=VECTOR('',#11602,1.2);
#3450=VECTOR('',#11609,1.);
#3451=VECTOR('',#11612,1.);
#3452=VECTOR('',#11617,1.);
#3453=VECTOR('',#11620,1.);
#3454=VECTOR('',#11625,1.);
#3455=VECTOR('',#11628,1.);
#3456=VECTOR('',#11633,1.);
#3457=VECTOR('',#11636,1.);
#3458=VECTOR('',#11669,1.59);
#3459=VECTOR('',#11680,1.2);
#3460=VECTOR('',#11687,1.);
#3461=VECTOR('',#11688,1.);
#3462=VECTOR('',#11689,1.);
#3463=VECTOR('',#11690,1.);
#3464=VECTOR('',#11693,1.);
#3465=VECTOR('',#11694,1.);
#3466=VECTOR('',#11695,1.);
#3467=VECTOR('',#11696,1.);
#3468=VECTOR('',#11699,1.);
#3469=VECTOR('',#11702,1.);
#3470=VECTOR('',#11719,1.);
#3471=VECTOR('',#11722,1.);
#3472=VECTOR('',#11725,1.);
#3473=VECTOR('',#11726,1.);
#3474=VECTOR('',#11729,1.);
#3475=VECTOR('',#11730,1.);
#3476=VECTOR('',#11755,0.976185);
#3477=VECTOR('',#11762,0.5);
#3478=VECTOR('',#11767,0.53);
#3479=VECTOR('',#11776,0.976185);
#3480=VECTOR('',#11783,0.53);
#3481=VECTOR('',#11802,1.023815);
#3482=VECTOR('',#11813,1.47);
#3483=VECTOR('',#11818,1.5);
#3484=VECTOR('',#11823,1.47);
#3485=VECTOR('',#11828,1.023815);
#3486=VECTOR('',#11879,1.019052);
#3487=VECTOR('',#11956,0.980948);
#3488=VECTOR('',#11985,1.013815);
#3489=VECTOR('',#11992,0.991185);
#3490=VECTOR('',#12003,1.013815);
#3491=VECTOR('',#12010,0.991185);
#3492=VECTOR('',#12025,1.);
#3493=VECTOR('',#12026,1.);
#3494=VECTOR('',#12027,1.);
#3495=VECTOR('',#12028,1.);
#3496=VECTOR('',#12031,1.);
#3497=VECTOR('',#12032,1.);
#3498=VECTOR('',#12033,1.);
#3499=VECTOR('',#12036,1.);
#3500=VECTOR('',#12037,1.);
#3501=VECTOR('',#12038,1.);
#3502=VECTOR('',#12041,1.);
#3503=VECTOR('',#12042,1.);
#3504=VECTOR('',#12043,1.);
#3505=VECTOR('',#12046,1.);
#3506=VECTOR('',#12047,1.);
#3507=VECTOR('',#12048,1.);
#3508=VECTOR('',#12051,1.);
#3509=VECTOR('',#12052,1.);
#3510=VECTOR('',#12065,0.2);
#3511=VECTOR('',#12078,0.325);
#3512=VECTOR('',#12083,0.35);
#3513=VECTOR('',#12088,0.335);
#3514=VECTOR('',#12097,0.21);
#3515=VECTOR('',#12102,0.2);
#3516=VECTOR('',#12105,0.18);
#3517=VECTOR('',#12124,1.070235);
#3518=VECTOR('',#12131,0.6);
#3519=VECTOR('',#12136,0.63);
#3520=VECTOR('',#12145,1.070235);
#3521=VECTOR('',#12152,0.63);
#3522=VECTOR('',#12171,1.129765);
#3523=VECTOR('',#12182,1.57);
#3524=VECTOR('',#12187,1.6);
#3525=VECTOR('',#12192,1.57);
#3526=VECTOR('',#12197,1.129765);
#3527=VECTOR('',#12244,1.123812);
#3528=VECTOR('',#12313,1.076188);
#3529=VECTOR('',#12342,1.119765);
#3530=VECTOR('',#12349,1.085235);
#3531=VECTOR('',#12360,1.119765);
#3532=VECTOR('',#12367,1.085235);
#3533=VECTOR('',#12382,1.);
#3534=VECTOR('',#12383,1.);
#3535=VECTOR('',#12384,1.);
#3536=VECTOR('',#12385,1.);
#3537=VECTOR('',#12388,1.);
#3538=VECTOR('',#12389,1.);
#3539=VECTOR('',#12390,1.);
#3540=VECTOR('',#12393,1.);
#3541=VECTOR('',#12394,1.);
#3542=VECTOR('',#12395,1.);
#3543=VECTOR('',#12398,1.);
#3544=VECTOR('',#12399,1.);
#3545=VECTOR('',#12400,1.);
#3546=VECTOR('',#12403,1.);
#3547=VECTOR('',#12404,1.);
#3548=VECTOR('',#12405,1.);
#3549=VECTOR('',#12408,1.);
#3550=VECTOR('',#12409,1.);
#3551=VECTOR('',#12426,0.325);
#3552=VECTOR('',#12431,0.35);
#3553=VECTOR('',#12436,0.335);
#3554=VECTOR('',#12445,0.21);
#3555=VECTOR('',#12448,0.2);
#3556=VECTOR('',#12457,0.165);
#3557=VECTOR('',#12476,0.7);
#3558=VECTOR('',#12479,0.5);
#3559=VECTOR('',#12486,0.4);
#3560=VECTOR('',#12495,0.5);
#3561=VECTOR('',#12506,0.505);
#3562=VECTOR('',#12515,0.405);
#3563=VECTOR('',#12522,0.7);
#3564=VECTOR('',#12535,0.505);
#3565=VECTOR('',#12542,0.7);
#3566=VECTOR('',#12555,0.15);
#3567=VECTOR('',#12568,0.15);
#3568=VECTOR('',#12581,0.225);
#3569=VECTOR('',#12588,0.6);
#3570=VECTOR('',#12599,0.125);
#3571=VECTOR('',#12602,0.125);
#3572=VECTOR('',#12607,0.65);
#3573=VECTOR('',#12608,0.65);
#3574=VECTOR('',#12613,0.125);
#3575=VECTOR('',#12616,0.125);
#3576=VECTOR('',#12621,0.4);
#3577=VECTOR('',#12622,0.4);
#3578=VECTOR('',#12715,0.8);
#3579=VECTOR('',#12806,0.8);
#3580=VECTOR('',#12811,1.);
#3581=VECTOR('',#12812,1.);
#3582=VECTOR('',#12815,1.);
#3583=VECTOR('',#12818,1.);
#3584=VECTOR('',#12821,1.);
#3585=VECTOR('',#12824,1.);
#3586=VECTOR('',#12827,1.);
#3587=VECTOR('',#12830,1.);
#3588=VECTOR('',#12833,1.);
#3589=VECTOR('',#12836,1.);
#3590=VECTOR('',#12839,1.);
#3591=VECTOR('',#12842,1.);
#3592=VECTOR('',#12845,1.);
#3593=VECTOR('',#12848,1.);
#3594=VECTOR('',#12851,1.);
#3595=VECTOR('',#12854,1.);
#3596=VECTOR('',#12857,1.);
#3597=VECTOR('',#12860,1.);
#3598=VECTOR('',#12863,1.);
#3599=VECTOR('',#12866,1.);
#3600=VECTOR('',#12869,1.);
#3601=VECTOR('',#12872,1.);
#3602=VECTOR('',#12875,1.);
#3603=VECTOR('',#12878,1.);
#3604=VECTOR('',#12881,1.);
#3605=VECTOR('',#12884,1.);
#3606=VECTOR('',#12887,1.);
#3607=VECTOR('',#12890,1.);
#3608=VECTOR('',#12893,1.);
#3609=VECTOR('',#12896,1.);
#3610=VECTOR('',#12899,1.);
#3611=VECTOR('',#12902,1.);
#3612=VECTOR('',#12905,1.);
#3613=VECTOR('',#12908,1.);
#3614=VECTOR('',#12911,1.);
#3615=VECTOR('',#12914,1.);
#3616=VECTOR('',#12917,1.);
#3617=VECTOR('',#12920,1.);
#3618=VECTOR('',#12923,1.);
#3619=VECTOR('',#12926,1.);
#3620=VECTOR('',#12937,0.165);
#3621=VECTOR('',#12956,0.8);
#3622=VECTOR('',#12959,0.6);
#3623=VECTOR('',#12968,0.6);
#3624=VECTOR('',#12977,0.605);
#3625=VECTOR('',#12984,0.8);
#3626=VECTOR('',#12997,0.605);
#3627=VECTOR('',#13004,0.8);
#3628=VECTOR('',#13017,0.15);
#3629=VECTOR('',#13030,0.15);
#3630=VECTOR('',#13043,0.225);
#3631=VECTOR('',#13050,0.8);
#3632=VECTOR('',#13061,0.125);
#3633=VECTOR('',#13064,0.125);
#3634=VECTOR('',#13069,1.);
#3635=VECTOR('',#13070,1.);
#3636=VECTOR('',#13075,0.125);
#3637=VECTOR('',#13078,0.125);
#3638=VECTOR('',#13083,0.6);
#3639=VECTOR('',#13084,0.6);
#3640=VECTOR('',#13257,1.4);
#3641=VECTOR('',#13428,1.4);
#3642=VECTOR('',#13433,1.);
#3643=VECTOR('',#13434,1.);
#3644=VECTOR('',#13437,1.);
#3645=VECTOR('',#13440,1.);
#3646=VECTOR('',#13443,1.);
#3647=VECTOR('',#13446,1.);
#3648=VECTOR('',#13449,1.);
#3649=VECTOR('',#13452,1.);
#3650=VECTOR('',#13455,1.);
#3651=VECTOR('',#13458,1.);
#3652=VECTOR('',#13461,1.);
#3653=VECTOR('',#13464,1.);
#3654=VECTOR('',#13467,1.);
#3655=VECTOR('',#13470,1.);
#3656=VECTOR('',#13473,1.);
#3657=VECTOR('',#13476,1.);
#3658=VECTOR('',#13479,1.);
#3659=VECTOR('',#13482,1.);
#3660=VECTOR('',#13485,1.);
#3661=VECTOR('',#13488,1.);
#3662=VECTOR('',#13491,1.);
#3663=VECTOR('',#13494,1.);
#3664=VECTOR('',#13497,1.);
#3665=VECTOR('',#13500,1.);
#3666=VECTOR('',#13503,1.);
#3667=VECTOR('',#13506,1.);
#3668=VECTOR('',#13509,1.);
#3669=VECTOR('',#13512,1.);
#3670=VECTOR('',#13515,1.);
#3671=VECTOR('',#13518,1.);
#3672=VECTOR('',#13521,1.);
#3673=VECTOR('',#13524,1.);
#3674=VECTOR('',#13527,1.);
#3675=VECTOR('',#13530,1.);
#3676=VECTOR('',#13533,1.);
#3677=VECTOR('',#13536,1.);
#3678=VECTOR('',#13539,1.);
#3679=VECTOR('',#13542,1.);
#3680=VECTOR('',#13545,1.);
#3681=VECTOR('',#13548,1.);
#3682=VECTOR('',#13551,1.);
#3683=VECTOR('',#13554,1.);
#3684=VECTOR('',#13557,1.);
#3685=VECTOR('',#13560,1.);
#3686=VECTOR('',#13563,1.);
#3687=VECTOR('',#13566,1.);
#3688=VECTOR('',#13569,1.);
#3689=VECTOR('',#13572,1.);
#3690=VECTOR('',#13575,1.);
#3691=VECTOR('',#13578,1.);
#3692=VECTOR('',#13581,1.);
#3693=VECTOR('',#13584,1.);
#3694=VECTOR('',#13587,1.);
#3695=VECTOR('',#13590,1.);
#3696=VECTOR('',#13593,1.);
#3697=VECTOR('',#13596,1.);
#3698=VECTOR('',#13599,1.);
#3699=VECTOR('',#13602,1.);
#3700=VECTOR('',#13605,1.);
#3701=VECTOR('',#13608,1.);
#3702=VECTOR('',#13611,1.);
#3703=VECTOR('',#13614,1.);
#3704=VECTOR('',#13617,1.);
#3705=VECTOR('',#13620,1.);
#3706=VECTOR('',#13623,1.);
#3707=VECTOR('',#13626,1.);
#3708=VECTOR('',#13629,1.);
#3709=VECTOR('',#13632,1.);
#3710=VECTOR('',#13635,1.);
#3711=VECTOR('',#13638,1.);
#3712=VECTOR('',#13641,1.);
#3713=VECTOR('',#13644,1.);
#3714=VECTOR('',#13647,1.);
#3715=VECTOR('',#13650,1.);
#3716=VECTOR('',#13653,1.);
#3717=VECTOR('',#13656,1.);
#3718=VECTOR('',#13659,1.);
#3719=VECTOR('',#13662,1.);
#3720=VECTOR('',#13665,1.);
#3721=VECTOR('',#13668,1.);
#3722=VECTOR('',#13681,0.325);
#3723=VECTOR('',#13686,0.35);
#3724=VECTOR('',#13691,0.335);
#3725=VECTOR('',#13700,0.21);
#3726=VECTOR('',#13705,0.2);
#3727=VECTOR('',#13710,0.18);
#3728=VECTOR('',#13715,1.);
#3729=VECTOR('',#13716,1.);
#3730=VECTOR('',#13717,1.);
#3731=VECTOR('',#13718,1.);
#3732=VECTOR('',#13721,1.);
#3733=VECTOR('',#13722,1.);
#3734=VECTOR('',#13723,1.);
#3735=VECTOR('',#13726,1.);
#3736=VECTOR('',#13727,1.);
#3737=VECTOR('',#13728,1.);
#3738=VECTOR('',#13731,1.);
#3739=VECTOR('',#13732,1.);
#3740=VECTOR('',#13733,1.);
#3741=VECTOR('',#13736,1.);
#3742=VECTOR('',#13737,1.);
#3743=VECTOR('',#13738,1.);
#3744=VECTOR('',#13741,1.);
#3745=VECTOR('',#13742,1.);
#3746=VERTEX_POINT('',#13877);
#3747=VERTEX_POINT('',#13878);
#3748=VERTEX_POINT('',#13880);
#3749=VERTEX_POINT('',#13882);
#3750=VERTEX_POINT('',#13886);
#3751=VERTEX_POINT('',#13887);
#3752=VERTEX_POINT('',#13889);
#3753=VERTEX_POINT('',#13891);
#3754=VERTEX_POINT('',#13895);
#3755=VERTEX_POINT('',#13896);
#3756=VERTEX_POINT('',#13898);
#3757=VERTEX_POINT('',#13900);
#3758=VERTEX_POINT('',#13903);
#3759=VERTEX_POINT('',#13904);
#3760=VERTEX_POINT('',#13906);
#3761=VERTEX_POINT('',#13908);
#3762=VERTEX_POINT('',#13911);
#3763=VERTEX_POINT('',#13912);
#3764=VERTEX_POINT('',#13914);
#3765=VERTEX_POINT('',#13916);
#3766=VERTEX_POINT('',#13919);
#3767=VERTEX_POINT('',#13920);
#3768=VERTEX_POINT('',#13922);
#3769=VERTEX_POINT('',#13924);
#3770=VERTEX_POINT('',#13934);
#3771=VERTEX_POINT('',#13936);
#3772=VERTEX_POINT('',#13940);
#3773=VERTEX_POINT('',#13942);
#3774=VERTEX_POINT('',#13950);
#3775=VERTEX_POINT('',#13951);
#3776=VERTEX_POINT('',#13953);
#3777=VERTEX_POINT('',#13956);
#3778=VERTEX_POINT('',#13958);
#3779=VERTEX_POINT('',#13960);
#3780=VERTEX_POINT('',#13964);
#3781=VERTEX_POINT('',#13966);
#3782=VERTEX_POINT('',#13974);
#3783=VERTEX_POINT('',#13975);
#3784=VERTEX_POINT('',#13977);
#3785=VERTEX_POINT('',#13980);
#3786=VERTEX_POINT('',#13982);
#3787=VERTEX_POINT('',#13984);
#3788=VERTEX_POINT('',#13988);
#3789=VERTEX_POINT('',#13990);
#3790=VERTEX_POINT('',#14002);
#3791=VERTEX_POINT('',#14004);
#3792=VERTEX_POINT('',#14009);
#3793=VERTEX_POINT('',#14011);
#3794=VERTEX_POINT('',#14020);
#3795=VERTEX_POINT('',#14022);
#3796=VERTEX_POINT('',#14026);
#3797=VERTEX_POINT('',#14030);
#3798=VERTEX_POINT('',#14038);
#3799=VERTEX_POINT('',#14039);
#3800=VERTEX_POINT('',#14041);
#3801=VERTEX_POINT('',#14043);
#3802=VERTEX_POINT('',#14047);
#3803=VERTEX_POINT('',#14049);
#3804=VERTEX_POINT('',#14053);
#3805=VERTEX_POINT('',#14055);
#3806=VERTEX_POINT('',#14065);
#3807=VERTEX_POINT('',#14066);
#3808=VERTEX_POINT('',#14068);
#3809=VERTEX_POINT('',#14070);
#3810=VERTEX_POINT('',#14074);
#3811=VERTEX_POINT('',#14076);
#3812=VERTEX_POINT('',#14080);
#3813=VERTEX_POINT('',#14082);
#3814=VERTEX_POINT('',#14092);
#3815=VERTEX_POINT('',#14094);
#3816=VERTEX_POINT('',#14098);
#3817=VERTEX_POINT('',#14100);
#3818=VERTEX_POINT('',#14104);
#3819=VERTEX_POINT('',#14106);
#3820=VERTEX_POINT('',#14110);
#3821=VERTEX_POINT('',#14112);
#3822=VERTEX_POINT('',#14116);
#3823=VERTEX_POINT('',#14118);
#3824=VERTEX_POINT('',#14122);
#3825=VERTEX_POINT('',#14124);
#3826=VERTEX_POINT('',#14128);
#3827=VERTEX_POINT('',#14130);
#3828=VERTEX_POINT('',#14134);
#3829=VERTEX_POINT('',#14136);
#3830=VERTEX_POINT('',#14140);
#3831=VERTEX_POINT('',#14142);
#3832=VERTEX_POINT('',#14146);
#3833=VERTEX_POINT('',#14147);
#3834=VERTEX_POINT('',#14149);
#3835=VERTEX_POINT('',#14151);
#3836=VERTEX_POINT('',#14155);
#3837=VERTEX_POINT('',#14156);
#3838=VERTEX_POINT('',#14158);
#3839=VERTEX_POINT('',#14160);
#3840=VERTEX_POINT('',#14164);
#3841=VERTEX_POINT('',#14166);
#3842=VERTEX_POINT('',#14170);
#3843=VERTEX_POINT('',#14172);
#3844=VERTEX_POINT('',#14176);
#3845=VERTEX_POINT('',#14178);
#3846=VERTEX_POINT('',#14183);
#3847=VERTEX_POINT('',#14187);
#3848=VERTEX_POINT('',#14197);
#3849=VERTEX_POINT('',#14199);
#3850=VERTEX_POINT('',#14203);
#3851=VERTEX_POINT('',#14205);
#3852=VERTEX_POINT('',#14212);
#3853=VERTEX_POINT('',#14213);
#3854=VERTEX_POINT('',#14215);
#3855=VERTEX_POINT('',#14217);
#3856=VERTEX_POINT('',#14221);
#3857=VERTEX_POINT('',#14222);
#3858=VERTEX_POINT('',#14224);
#3859=VERTEX_POINT('',#14226);
#3860=VERTEX_POINT('',#14230);
#3861=VERTEX_POINT('',#14231);
#3862=VERTEX_POINT('',#14233);
#3863=VERTEX_POINT('',#14235);
#3864=VERTEX_POINT('',#14239);
#3865=VERTEX_POINT('',#14240);
#3866=VERTEX_POINT('',#14242);
#3867=VERTEX_POINT('',#14244);
#3868=VERTEX_POINT('',#14252);
#3869=VERTEX_POINT('',#14263);
#3870=VERTEX_POINT('',#14265);
#3871=VERTEX_POINT('',#14269);
#3872=VERTEX_POINT('',#14276);
#3873=VERTEX_POINT('',#14277);
#3874=VERTEX_POINT('',#14279);
#3875=VERTEX_POINT('',#14281);
#3876=VERTEX_POINT('',#14285);
#3877=VERTEX_POINT('',#14286);
#3878=VERTEX_POINT('',#14288);
#3879=VERTEX_POINT('',#14290);
#3880=VERTEX_POINT('',#14294);
#3881=VERTEX_POINT('',#14295);
#3882=VERTEX_POINT('',#14297);
#3883=VERTEX_POINT('',#14299);
#3884=VERTEX_POINT('',#14303);
#3885=VERTEX_POINT('',#14304);
#3886=VERTEX_POINT('',#14306);
#3887=VERTEX_POINT('',#14308);
#3888=VERTEX_POINT('',#14316);
#3889=VERTEX_POINT('',#14327);
#3890=VERTEX_POINT('',#14331);
#3891=VERTEX_POINT('',#14334);
#3892=VERTEX_POINT('',#14340);
#3893=VERTEX_POINT('',#14342);
#3894=VERTEX_POINT('',#14346);
#3895=VERTEX_POINT('',#14348);
#3896=VERTEX_POINT('',#14352);
#3897=VERTEX_POINT('',#14354);
#3898=VERTEX_POINT('',#14358);
#3899=VERTEX_POINT('',#14360);
#3900=VERTEX_POINT('',#14364);
#3901=VERTEX_POINT('',#14366);
#3902=VERTEX_POINT('',#14370);
#3903=VERTEX_POINT('',#14372);
#3904=VERTEX_POINT('',#14376);
#3905=VERTEX_POINT('',#14378);
#3906=VERTEX_POINT('',#14382);
#3907=VERTEX_POINT('',#14384);
#3908=VERTEX_POINT('',#14388);
#3909=VERTEX_POINT('',#14390);
#3910=VERTEX_POINT('',#14394);
#3911=VERTEX_POINT('',#14395);
#3912=VERTEX_POINT('',#14397);
#3913=VERTEX_POINT('',#14399);
#3914=VERTEX_POINT('',#14403);
#3915=VERTEX_POINT('',#14404);
#3916=VERTEX_POINT('',#14406);
#3917=VERTEX_POINT('',#14408);
#3918=VERTEX_POINT('',#14412);
#3919=VERTEX_POINT('',#14414);
#3920=VERTEX_POINT('',#14418);
#3921=VERTEX_POINT('',#14420);
#3922=VERTEX_POINT('',#14424);
#3923=VERTEX_POINT('',#14426);
#3924=VERTEX_POINT('',#14431);
#3925=VERTEX_POINT('',#14435);
#3926=VERTEX_POINT('',#14445);
#3927=VERTEX_POINT('',#14447);
#3928=VERTEX_POINT('',#14451);
#3929=VERTEX_POINT('',#14453);
#3930=VERTEX_POINT('',#14460);
#3931=VERTEX_POINT('',#14462);
#3932=VERTEX_POINT('',#14466);
#3933=VERTEX_POINT('',#14468);
#3934=VERTEX_POINT('',#14475);
#3935=VERTEX_POINT('',#14477);
#3936=VERTEX_POINT('',#14481);
#3937=VERTEX_POINT('',#14483);
#3938=VERTEX_POINT('',#14490);
#3939=VERTEX_POINT('',#14492);
#3940=VERTEX_POINT('',#14496);
#3941=VERTEX_POINT('',#14498);
#3942=VERTEX_POINT('',#14505);
#3943=VERTEX_POINT('',#14507);
#3944=VERTEX_POINT('',#14511);
#3945=VERTEX_POINT('',#14513);
#3946=VERTEX_POINT('',#14520);
#3947=VERTEX_POINT('',#14521);
#3948=VERTEX_POINT('',#14523);
#3949=VERTEX_POINT('',#14525);
#3950=VERTEX_POINT('',#14529);
#3951=VERTEX_POINT('',#14530);
#3952=VERTEX_POINT('',#14532);
#3953=VERTEX_POINT('',#14534);
#3954=VERTEX_POINT('',#14538);
#3955=VERTEX_POINT('',#14539);
#3956=VERTEX_POINT('',#14541);
#3957=VERTEX_POINT('',#14543);
#3958=VERTEX_POINT('',#14547);
#3959=VERTEX_POINT('',#14548);
#3960=VERTEX_POINT('',#14550);
#3961=VERTEX_POINT('',#14552);
#3962=VERTEX_POINT('',#14560);
#3963=VERTEX_POINT('',#14571);
#3964=VERTEX_POINT('',#14573);
#3965=VERTEX_POINT('',#14577);
#3966=VERTEX_POINT('',#14584);
#3967=VERTEX_POINT('',#14585);
#3968=VERTEX_POINT('',#14587);
#3969=VERTEX_POINT('',#14589);
#3970=VERTEX_POINT('',#14593);
#3971=VERTEX_POINT('',#14594);
#3972=VERTEX_POINT('',#14596);
#3973=VERTEX_POINT('',#14598);
#3974=VERTEX_POINT('',#14602);
#3975=VERTEX_POINT('',#14603);
#3976=VERTEX_POINT('',#14605);
#3977=VERTEX_POINT('',#14607);
#3978=VERTEX_POINT('',#14611);
#3979=VERTEX_POINT('',#14612);
#3980=VERTEX_POINT('',#14614);
#3981=VERTEX_POINT('',#14616);
#3982=VERTEX_POINT('',#14624);
#3983=VERTEX_POINT('',#14635);
#3984=VERTEX_POINT('',#14639);
#3985=VERTEX_POINT('',#14642);
#3986=VERTEX_POINT('',#14648);
#3987=VERTEX_POINT('',#14649);
#3988=VERTEX_POINT('',#14651);
#3989=VERTEX_POINT('',#14653);
#3990=VERTEX_POINT('',#14657);
#3991=VERTEX_POINT('',#14658);
#3992=VERTEX_POINT('',#14660);
#3993=VERTEX_POINT('',#14662);
#3994=VERTEX_POINT('',#14666);
#3995=VERTEX_POINT('',#14667);
#3996=VERTEX_POINT('',#14669);
#3997=VERTEX_POINT('',#14671);
#3998=VERTEX_POINT('',#14681);
#3999=VERTEX_POINT('',#14683);
#4000=VERTEX_POINT('',#14687);
#4001=VERTEX_POINT('',#14691);
#4002=VERTEX_POINT('',#14700);
#4003=VERTEX_POINT('',#14701);
#4004=VERTEX_POINT('',#14704);
#4005=VERTEX_POINT('',#14706);
#4006=VERTEX_POINT('',#14710);
#4007=VERTEX_POINT('',#14714);
#4008=VERTEX_POINT('',#14716);
#4009=VERTEX_POINT('',#14720);
#4010=VERTEX_POINT('',#14725);
#4011=VERTEX_POINT('',#14729);
#4012=VERTEX_POINT('',#14735);
#4013=VERTEX_POINT('',#14736);
#4014=VERTEX_POINT('',#14739);
#4015=VERTEX_POINT('',#14741);
#4016=VERTEX_POINT('',#14745);
#4017=VERTEX_POINT('',#14749);
#4018=VERTEX_POINT('',#14751);
#4019=VERTEX_POINT('',#14754);
#4020=VERTEX_POINT('',#14758);
#4021=VERTEX_POINT('',#14762);
#4022=VERTEX_POINT('',#14770);
#4023=VERTEX_POINT('',#14771);
#4024=VERTEX_POINT('',#14774);
#4025=VERTEX_POINT('',#14775);
#4026=VERTEX_POINT('',#14778);
#4027=VERTEX_POINT('',#14779);
#4028=VERTEX_POINT('',#14782);
#4029=VERTEX_POINT('',#14783);
#4030=VERTEX_POINT('',#14786);
#4031=VERTEX_POINT('',#14787);
#4032=VERTEX_POINT('',#14790);
#4033=VERTEX_POINT('',#14791);
#4034=VERTEX_POINT('',#14794);
#4035=VERTEX_POINT('',#14795);
#4036=VERTEX_POINT('',#14798);
#4037=VERTEX_POINT('',#14799);
#4038=VERTEX_POINT('',#14803);
#4039=VERTEX_POINT('',#14804);
#4040=VERTEX_POINT('',#14827);
#4041=VERTEX_POINT('',#14829);
#4042=VERTEX_POINT('',#14854);
#4043=VERTEX_POINT('',#14856);
#4044=VERTEX_POINT('',#14879);
#4045=VERTEX_POINT('',#14881);
#4046=VERTEX_POINT('',#14904);
#4047=VERTEX_POINT('',#14906);
#4048=VERTEX_POINT('',#14919);
#4049=VERTEX_POINT('',#14922);
#4050=VERTEX_POINT('',#14935);
#4051=VERTEX_POINT('',#14937);
#4052=VERTEX_POINT('',#14960);
#4053=VERTEX_POINT('',#14962);
#4054=VERTEX_POINT('',#14985);
#4055=VERTEX_POINT('',#14987);
#4056=VERTEX_POINT('',#15010);
#4057=VERTEX_POINT('',#15012);
#4058=VERTEX_POINT('',#15037);
#4059=VERTEX_POINT('',#15041);
#4060=VERTEX_POINT('',#15066);
#4061=VERTEX_POINT('',#15070);
#4062=VERTEX_POINT('',#15095);
#4063=VERTEX_POINT('',#15099);
#4064=VERTEX_POINT('',#15100);
#4065=VERTEX_POINT('',#15127);
#4066=VERTEX_POINT('',#15131);
#4067=VERTEX_POINT('',#15156);
#4068=VERTEX_POINT('',#15160);
#4069=VERTEX_POINT('',#15185);
#4070=VERTEX_POINT('',#15189);
#4071=VERTEX_POINT('',#15214);
#4072=VERTEX_POINT('',#15217);
#4073=VERTEX_POINT('',#15219);
#4074=VERTEX_POINT('',#15251);
#4075=VERTEX_POINT('',#15253);
#4076=VERTEX_POINT('',#15256);
#4077=VERTEX_POINT('',#15260);
#4078=VERTEX_POINT('',#15265);
#4079=VERTEX_POINT('',#15267);
#4080=VERTEX_POINT('',#15270);
#4081=VERTEX_POINT('',#15274);
#4082=VERTEX_POINT('',#15285);
#4083=VERTEX_POINT('',#15286);
#4084=VERTEX_POINT('',#15288);
#4085=VERTEX_POINT('',#15290);
#4086=VERTEX_POINT('',#15294);
#4087=VERTEX_POINT('',#15296);
#4088=VERTEX_POINT('',#15300);
#4089=VERTEX_POINT('',#15302);
#4090=VERTEX_POINT('',#15306);
#4091=VERTEX_POINT('',#15308);
#4092=VERTEX_POINT('',#15312);
#4093=VERTEX_POINT('',#15314);
#4094=VERTEX_POINT('',#15323);
#4095=VERTEX_POINT('',#15325);
#4096=VERTEX_POINT('',#15328);
#4097=VERTEX_POINT('',#15333);
#4098=VERTEX_POINT('',#15336);
#4099=VERTEX_POINT('',#15340);
#4100=VERTEX_POINT('',#15344);
#4101=VERTEX_POINT('',#15348);
#4102=VERTEX_POINT('',#15351);
#4103=VERTEX_POINT('',#15355);
#4104=VERTEX_POINT('',#15363);
#4105=VERTEX_POINT('',#15364);
#4106=VERTEX_POINT('',#15367);
#4107=VERTEX_POINT('',#15369);
#4108=VERTEX_POINT('',#15373);
#4109=VERTEX_POINT('',#15377);
#4110=VERTEX_POINT('',#15379);
#4111=VERTEX_POINT('',#15383);
#4112=VERTEX_POINT('',#15388);
#4113=VERTEX_POINT('',#15392);
#4114=VERTEX_POINT('',#15398);
#4115=VERTEX_POINT('',#15399);
#4116=VERTEX_POINT('',#15402);
#4117=VERTEX_POINT('',#15404);
#4118=VERTEX_POINT('',#15408);
#4119=VERTEX_POINT('',#15412);
#4120=VERTEX_POINT('',#15414);
#4121=VERTEX_POINT('',#15417);
#4122=VERTEX_POINT('',#15421);
#4123=VERTEX_POINT('',#15425);
#4124=VERTEX_POINT('',#15433);
#4125=VERTEX_POINT('',#15434);
#4126=VERTEX_POINT('',#15437);
#4127=VERTEX_POINT('',#15438);
#4128=VERTEX_POINT('',#15441);
#4129=VERTEX_POINT('',#15442);
#4130=VERTEX_POINT('',#15445);
#4131=VERTEX_POINT('',#15446);
#4132=VERTEX_POINT('',#15449);
#4133=VERTEX_POINT('',#15450);
#4134=VERTEX_POINT('',#15453);
#4135=VERTEX_POINT('',#15454);
#4136=VERTEX_POINT('',#15457);
#4137=VERTEX_POINT('',#15458);
#4138=VERTEX_POINT('',#15462);
#4139=VERTEX_POINT('',#15463);
#4140=VERTEX_POINT('',#15486);
#4141=VERTEX_POINT('',#15488);
#4142=VERTEX_POINT('',#15513);
#4143=VERTEX_POINT('',#15515);
#4144=VERTEX_POINT('',#15538);
#4145=VERTEX_POINT('',#15540);
#4146=VERTEX_POINT('',#15563);
#4147=VERTEX_POINT('',#15565);
#4148=VERTEX_POINT('',#15568);
#4149=VERTEX_POINT('',#15570);
#4150=VERTEX_POINT('',#15593);
#4151=VERTEX_POINT('',#15595);
#4152=VERTEX_POINT('',#15618);
#4153=VERTEX_POINT('',#15620);
#4154=VERTEX_POINT('',#15643);
#4155=VERTEX_POINT('',#15645);
#4156=VERTEX_POINT('',#15670);
#4157=VERTEX_POINT('',#15674);
#4158=VERTEX_POINT('',#15699);
#4159=VERTEX_POINT('',#15703);
#4160=VERTEX_POINT('',#15728);
#4161=VERTEX_POINT('',#15730);
#4162=VERTEX_POINT('',#15734);
#4163=VERTEX_POINT('',#15759);
#4164=VERTEX_POINT('',#15763);
#4165=VERTEX_POINT('',#15788);
#4166=VERTEX_POINT('',#15792);
#4167=VERTEX_POINT('',#15817);
#4168=VERTEX_POINT('',#15820);
#4169=VERTEX_POINT('',#15822);
#4170=VERTEX_POINT('',#15854);
#4171=VERTEX_POINT('',#15856);
#4172=VERTEX_POINT('',#15859);
#4173=VERTEX_POINT('',#15863);
#4174=VERTEX_POINT('',#15868);
#4175=VERTEX_POINT('',#15870);
#4176=VERTEX_POINT('',#15873);
#4177=VERTEX_POINT('',#15877);
#4178=VERTEX_POINT('',#15888);
#4179=VERTEX_POINT('',#15889);
#4180=VERTEX_POINT('',#15891);
#4181=VERTEX_POINT('',#15893);
#4182=VERTEX_POINT('',#15897);
#4183=VERTEX_POINT('',#15899);
#4184=VERTEX_POINT('',#15903);
#4185=VERTEX_POINT('',#15905);
#4186=VERTEX_POINT('',#15909);
#4187=VERTEX_POINT('',#15911);
#4188=VERTEX_POINT('',#15915);
#4189=VERTEX_POINT('',#15917);
#4190=VERTEX_POINT('',#15926);
#4191=VERTEX_POINT('',#15929);
#4192=VERTEX_POINT('',#15932);
#4193=VERTEX_POINT('',#15936);
#4194=VERTEX_POINT('',#15940);
#4195=VERTEX_POINT('',#15944);
#4196=VERTEX_POINT('',#15947);
#4197=VERTEX_POINT('',#15955);
#4198=VERTEX_POINT('',#15957);
#4199=VERTEX_POINT('',#15962);
#4200=VERTEX_POINT('',#15964);
#4201=VERTEX_POINT('',#15967);
#4202=VERTEX_POINT('',#15969);
#4203=VERTEX_POINT('',#15974);
#4204=VERTEX_POINT('',#15978);
#4205=VERTEX_POINT('',#15980);
#4206=VERTEX_POINT('',#15985);
#4207=VERTEX_POINT('',#15992);
#4208=VERTEX_POINT('',#15994);
#4209=VERTEX_POINT('',#15998);
#4210=VERTEX_POINT('',#16001);
#4211=VERTEX_POINT('',#16005);
#4212=VERTEX_POINT('',#16007);
#4213=VERTEX_POINT('',#16014);
#4214=VERTEX_POINT('',#16016);
#4215=VERTEX_POINT('',#16020);
#4216=VERTEX_POINT('',#16022);
#4217=VERTEX_POINT('',#16029);
#4218=VERTEX_POINT('',#16031);
#4219=VERTEX_POINT('',#16038);
#4220=VERTEX_POINT('',#16040);
#4221=VERTEX_POINT('',#16047);
#4222=VERTEX_POINT('',#16049);
#4223=VERTEX_POINT('',#16053);
#4224=VERTEX_POINT('',#16055);
#4225=VERTEX_POINT('',#16062);
#4226=VERTEX_POINT('',#16063);
#4227=VERTEX_POINT('',#16074);
#4228=VERTEX_POINT('',#16103);
#4229=VERTEX_POINT('',#16105);
#4230=VERTEX_POINT('',#16116);
#4231=VERTEX_POINT('',#16127);
#4232=VERTEX_POINT('',#16149);
#4233=VERTEX_POINT('',#16150);
#4234=VERTEX_POINT('',#16187);
#4235=VERTEX_POINT('',#16189);
#4236=VERTEX_POINT('',#16200);
#4237=VERTEX_POINT('',#16230);
#4238=VERTEX_POINT('',#16233);
#4239=VERTEX_POINT('',#16236);
#4240=VERTEX_POINT('',#16237);
#4241=VERTEX_POINT('',#16256);
#4242=VERTEX_POINT('',#16277);
#4243=VERTEX_POINT('',#16278);
#4244=VERTEX_POINT('',#16297);
#4245=VERTEX_POINT('',#16319);
#4246=VERTEX_POINT('',#16321);
#4247=VERTEX_POINT('',#16359);
#4248=VERTEX_POINT('',#16360);
#4249=VERTEX_POINT('',#16399);
#4250=VERTEX_POINT('',#16402);
#4251=VERTEX_POINT('',#16407);
#4252=VERTEX_POINT('',#16409);
#4253=VERTEX_POINT('',#16410);
#4254=VERTEX_POINT('',#16412);
#4255=VERTEX_POINT('',#16414);
#4256=VERTEX_POINT('',#16416);
#4257=VERTEX_POINT('',#16418);
#4258=VERTEX_POINT('',#16420);
#4259=VERTEX_POINT('',#16422);
#4260=VERTEX_POINT('',#16424);
#4261=VERTEX_POINT('',#16426);
#4262=VERTEX_POINT('',#16428);
#4263=VERTEX_POINT('',#16430);
#4264=VERTEX_POINT('',#16432);
#4265=VERTEX_POINT('',#16434);
#4266=VERTEX_POINT('',#16436);
#4267=VERTEX_POINT('',#16438);
#4268=VERTEX_POINT('',#16440);
#4269=VERTEX_POINT('',#16442);
#4270=VERTEX_POINT('',#16444);
#4271=VERTEX_POINT('',#16446);
#4272=VERTEX_POINT('',#16448);
#4273=VERTEX_POINT('',#16450);
#4274=VERTEX_POINT('',#16452);
#4275=VERTEX_POINT('',#16454);
#4276=VERTEX_POINT('',#16456);
#4277=VERTEX_POINT('',#16458);
#4278=VERTEX_POINT('',#16460);
#4279=VERTEX_POINT('',#16462);
#4280=VERTEX_POINT('',#16464);
#4281=VERTEX_POINT('',#16466);
#4282=VERTEX_POINT('',#16468);
#4283=VERTEX_POINT('',#16470);
#4284=VERTEX_POINT('',#16472);
#4285=VERTEX_POINT('',#16474);
#4286=VERTEX_POINT('',#16476);
#4287=VERTEX_POINT('',#16478);
#4288=VERTEX_POINT('',#16480);
#4289=VERTEX_POINT('',#16482);
#4290=VERTEX_POINT('',#16484);
#4291=VERTEX_POINT('',#16486);
#4292=VERTEX_POINT('',#16490);
#4293=VERTEX_POINT('',#16495);
#4294=VERTEX_POINT('',#16497);
#4295=VERTEX_POINT('',#16498);
#4296=VERTEX_POINT('',#16500);
#4297=VERTEX_POINT('',#16502);
#4298=VERTEX_POINT('',#16504);
#4299=VERTEX_POINT('',#16506);
#4300=VERTEX_POINT('',#16508);
#4301=VERTEX_POINT('',#16510);
#4302=VERTEX_POINT('',#16512);
#4303=VERTEX_POINT('',#16514);
#4304=VERTEX_POINT('',#16516);
#4305=VERTEX_POINT('',#16518);
#4306=VERTEX_POINT('',#16520);
#4307=VERTEX_POINT('',#16522);
#4308=VERTEX_POINT('',#16524);
#4309=VERTEX_POINT('',#16526);
#4310=VERTEX_POINT('',#16528);
#4311=VERTEX_POINT('',#16530);
#4312=VERTEX_POINT('',#16532);
#4313=VERTEX_POINT('',#16534);
#4314=VERTEX_POINT('',#16536);
#4315=VERTEX_POINT('',#16538);
#4316=VERTEX_POINT('',#16540);
#4317=VERTEX_POINT('',#16542);
#4318=VERTEX_POINT('',#16544);
#4319=VERTEX_POINT('',#16546);
#4320=VERTEX_POINT('',#16548);
#4321=VERTEX_POINT('',#16550);
#4322=VERTEX_POINT('',#16552);
#4323=VERTEX_POINT('',#16554);
#4324=VERTEX_POINT('',#16556);
#4325=VERTEX_POINT('',#16558);
#4326=VERTEX_POINT('',#16560);
#4327=VERTEX_POINT('',#16562);
#4328=VERTEX_POINT('',#16564);
#4329=VERTEX_POINT('',#16566);
#4330=VERTEX_POINT('',#16568);
#4331=VERTEX_POINT('',#16570);
#4332=VERTEX_POINT('',#16572);
#4333=VERTEX_POINT('',#16574);
#4334=VERTEX_POINT('',#16578);
#4335=VERTEX_POINT('',#16665);
#4336=VERTEX_POINT('',#16667);
#4337=VERTEX_POINT('',#16672);
#4338=VERTEX_POINT('',#16674);
#4339=VERTEX_POINT('',#16677);
#4340=VERTEX_POINT('',#16679);
#4341=VERTEX_POINT('',#16684);
#4342=VERTEX_POINT('',#16689);
#4343=VERTEX_POINT('',#16695);
#4344=VERTEX_POINT('',#16697);
#4345=VERTEX_POINT('',#16701);
#4346=VERTEX_POINT('',#16703);
#4347=VERTEX_POINT('',#16710);
#4348=VERTEX_POINT('',#16712);
#4349=VERTEX_POINT('',#16716);
#4350=VERTEX_POINT('',#16718);
#4351=VERTEX_POINT('',#16725);
#4352=VERTEX_POINT('',#16727);
#4353=VERTEX_POINT('',#16734);
#4354=VERTEX_POINT('',#16736);
#4355=VERTEX_POINT('',#16743);
#4356=VERTEX_POINT('',#16745);
#4357=VERTEX_POINT('',#16749);
#4358=VERTEX_POINT('',#16751);
#4359=VERTEX_POINT('',#16758);
#4360=VERTEX_POINT('',#16759);
#4361=VERTEX_POINT('',#16770);
#4362=VERTEX_POINT('',#16799);
#4363=VERTEX_POINT('',#16801);
#4364=VERTEX_POINT('',#16812);
#4365=VERTEX_POINT('',#16823);
#4366=VERTEX_POINT('',#16845);
#4367=VERTEX_POINT('',#16846);
#4368=VERTEX_POINT('',#16883);
#4369=VERTEX_POINT('',#16885);
#4370=VERTEX_POINT('',#16896);
#4371=VERTEX_POINT('',#16926);
#4372=VERTEX_POINT('',#16929);
#4373=VERTEX_POINT('',#16932);
#4374=VERTEX_POINT('',#16933);
#4375=VERTEX_POINT('',#16952);
#4376=VERTEX_POINT('',#16973);
#4377=VERTEX_POINT('',#16974);
#4378=VERTEX_POINT('',#16993);
#4379=VERTEX_POINT('',#17015);
#4380=VERTEX_POINT('',#17017);
#4381=VERTEX_POINT('',#17055);
#4382=VERTEX_POINT('',#17056);
#4383=VERTEX_POINT('',#17095);
#4384=VERTEX_POINT('',#17098);
#4385=VERTEX_POINT('',#17103);
#4386=VERTEX_POINT('',#17105);
#4387=VERTEX_POINT('',#17106);
#4388=VERTEX_POINT('',#17108);
#4389=VERTEX_POINT('',#17110);
#4390=VERTEX_POINT('',#17112);
#4391=VERTEX_POINT('',#17114);
#4392=VERTEX_POINT('',#17116);
#4393=VERTEX_POINT('',#17118);
#4394=VERTEX_POINT('',#17120);
#4395=VERTEX_POINT('',#17122);
#4396=VERTEX_POINT('',#17124);
#4397=VERTEX_POINT('',#17126);
#4398=VERTEX_POINT('',#17128);
#4399=VERTEX_POINT('',#17130);
#4400=VERTEX_POINT('',#17132);
#4401=VERTEX_POINT('',#17134);
#4402=VERTEX_POINT('',#17136);
#4403=VERTEX_POINT('',#17138);
#4404=VERTEX_POINT('',#17140);
#4405=VERTEX_POINT('',#17142);
#4406=VERTEX_POINT('',#17144);
#4407=VERTEX_POINT('',#17146);
#4408=VERTEX_POINT('',#17148);
#4409=VERTEX_POINT('',#17150);
#4410=VERTEX_POINT('',#17152);
#4411=VERTEX_POINT('',#17154);
#4412=VERTEX_POINT('',#17156);
#4413=VERTEX_POINT('',#17158);
#4414=VERTEX_POINT('',#17160);
#4415=VERTEX_POINT('',#17162);
#4416=VERTEX_POINT('',#17164);
#4417=VERTEX_POINT('',#17166);
#4418=VERTEX_POINT('',#17168);
#4419=VERTEX_POINT('',#17170);
#4420=VERTEX_POINT('',#17172);
#4421=VERTEX_POINT('',#17174);
#4422=VERTEX_POINT('',#17176);
#4423=VERTEX_POINT('',#17178);
#4424=VERTEX_POINT('',#17180);
#4425=VERTEX_POINT('',#17182);
#4426=VERTEX_POINT('',#17184);
#4427=VERTEX_POINT('',#17186);
#4428=VERTEX_POINT('',#17188);
#4429=VERTEX_POINT('',#17190);
#4430=VERTEX_POINT('',#17192);
#4431=VERTEX_POINT('',#17194);
#4432=VERTEX_POINT('',#17196);
#4433=VERTEX_POINT('',#17198);
#4434=VERTEX_POINT('',#17200);
#4435=VERTEX_POINT('',#17202);
#4436=VERTEX_POINT('',#17204);
#4437=VERTEX_POINT('',#17206);
#4438=VERTEX_POINT('',#17208);
#4439=VERTEX_POINT('',#17210);
#4440=VERTEX_POINT('',#17212);
#4441=VERTEX_POINT('',#17214);
#4442=VERTEX_POINT('',#17216);
#4443=VERTEX_POINT('',#17218);
#4444=VERTEX_POINT('',#17220);
#4445=VERTEX_POINT('',#17222);
#4446=VERTEX_POINT('',#17224);
#4447=VERTEX_POINT('',#17226);
#4448=VERTEX_POINT('',#17228);
#4449=VERTEX_POINT('',#17230);
#4450=VERTEX_POINT('',#17232);
#4451=VERTEX_POINT('',#17234);
#4452=VERTEX_POINT('',#17236);
#4453=VERTEX_POINT('',#17238);
#4454=VERTEX_POINT('',#17240);
#4455=VERTEX_POINT('',#17242);
#4456=VERTEX_POINT('',#17244);
#4457=VERTEX_POINT('',#17246);
#4458=VERTEX_POINT('',#17248);
#4459=VERTEX_POINT('',#17250);
#4460=VERTEX_POINT('',#17252);
#4461=VERTEX_POINT('',#17254);
#4462=VERTEX_POINT('',#17256);
#4463=VERTEX_POINT('',#17258);
#4464=VERTEX_POINT('',#17260);
#4465=VERTEX_POINT('',#17262);
#4466=VERTEX_POINT('',#17266);
#4467=VERTEX_POINT('',#17271);
#4468=VERTEX_POINT('',#17273);
#4469=VERTEX_POINT('',#17274);
#4470=VERTEX_POINT('',#17276);
#4471=VERTEX_POINT('',#17278);
#4472=VERTEX_POINT('',#17280);
#4473=VERTEX_POINT('',#17282);
#4474=VERTEX_POINT('',#17284);
#4475=VERTEX_POINT('',#17286);
#4476=VERTEX_POINT('',#17288);
#4477=VERTEX_POINT('',#17290);
#4478=VERTEX_POINT('',#17292);
#4479=VERTEX_POINT('',#17294);
#4480=VERTEX_POINT('',#17296);
#4481=VERTEX_POINT('',#17298);
#4482=VERTEX_POINT('',#17300);
#4483=VERTEX_POINT('',#17302);
#4484=VERTEX_POINT('',#17304);
#4485=VERTEX_POINT('',#17306);
#4486=VERTEX_POINT('',#17308);
#4487=VERTEX_POINT('',#17310);
#4488=VERTEX_POINT('',#17312);
#4489=VERTEX_POINT('',#17314);
#4490=VERTEX_POINT('',#17316);
#4491=VERTEX_POINT('',#17318);
#4492=VERTEX_POINT('',#17320);
#4493=VERTEX_POINT('',#17322);
#4494=VERTEX_POINT('',#17324);
#4495=VERTEX_POINT('',#17326);
#4496=VERTEX_POINT('',#17328);
#4497=VERTEX_POINT('',#17330);
#4498=VERTEX_POINT('',#17332);
#4499=VERTEX_POINT('',#17334);
#4500=VERTEX_POINT('',#17336);
#4501=VERTEX_POINT('',#17338);
#4502=VERTEX_POINT('',#17340);
#4503=VERTEX_POINT('',#17342);
#4504=VERTEX_POINT('',#17344);
#4505=VERTEX_POINT('',#17346);
#4506=VERTEX_POINT('',#17348);
#4507=VERTEX_POINT('',#17350);
#4508=VERTEX_POINT('',#17352);
#4509=VERTEX_POINT('',#17354);
#4510=VERTEX_POINT('',#17356);
#4511=VERTEX_POINT('',#17358);
#4512=VERTEX_POINT('',#17360);
#4513=VERTEX_POINT('',#17362);
#4514=VERTEX_POINT('',#17364);
#4515=VERTEX_POINT('',#17366);
#4516=VERTEX_POINT('',#17368);
#4517=VERTEX_POINT('',#17370);
#4518=VERTEX_POINT('',#17372);
#4519=VERTEX_POINT('',#17374);
#4520=VERTEX_POINT('',#17376);
#4521=VERTEX_POINT('',#17378);
#4522=VERTEX_POINT('',#17380);
#4523=VERTEX_POINT('',#17382);
#4524=VERTEX_POINT('',#17384);
#4525=VERTEX_POINT('',#17386);
#4526=VERTEX_POINT('',#17388);
#4527=VERTEX_POINT('',#17390);
#4528=VERTEX_POINT('',#17392);
#4529=VERTEX_POINT('',#17394);
#4530=VERTEX_POINT('',#17396);
#4531=VERTEX_POINT('',#17398);
#4532=VERTEX_POINT('',#17400);
#4533=VERTEX_POINT('',#17402);
#4534=VERTEX_POINT('',#17404);
#4535=VERTEX_POINT('',#17406);
#4536=VERTEX_POINT('',#17408);
#4537=VERTEX_POINT('',#17410);
#4538=VERTEX_POINT('',#17412);
#4539=VERTEX_POINT('',#17414);
#4540=VERTEX_POINT('',#17416);
#4541=VERTEX_POINT('',#17418);
#4542=VERTEX_POINT('',#17420);
#4543=VERTEX_POINT('',#17422);
#4544=VERTEX_POINT('',#17424);
#4545=VERTEX_POINT('',#17426);
#4546=VERTEX_POINT('',#17428);
#4547=VERTEX_POINT('',#17430);
#4548=VERTEX_POINT('',#17434);
#4549=VERTEX_POINT('',#17600);
#4550=VERTEX_POINT('',#17603);
#4551=VERTEX_POINT('',#17607);
#4552=VERTEX_POINT('',#17611);
#4553=VERTEX_POINT('',#17615);
#4554=VERTEX_POINT('',#17618);
#4555=VERTEX_POINT('',#17622);
#4556=VERTEX_POINT('',#17626);
#4557=VERTEX_POINT('',#17631);
#4558=VERTEX_POINT('',#17632);
#4559=VERTEX_POINT('',#17634);
#4560=VERTEX_POINT('',#17636);
#4561=VERTEX_POINT('',#17640);
#4562=VERTEX_POINT('',#17642);
#4563=VERTEX_POINT('',#17646);
#4564=VERTEX_POINT('',#17648);
#4565=VERTEX_POINT('',#17652);
#4566=VERTEX_POINT('',#17654);
#4567=VERTEX_POINT('',#17658);
#4568=VERTEX_POINT('',#17660);
#4569=EDGE_CURVE('',#3746,#3747,#2790,.T.);
#4570=EDGE_CURVE('',#3748,#3746,#2140,.T.);
#4571=EDGE_CURVE('',#3748,#3749,#2791,.T.);
#4572=EDGE_CURVE('',#3747,#3749,#2141,.T.);
#4573=EDGE_CURVE('',#3750,#3751,#2792,.T.);
#4574=EDGE_CURVE('',#3752,#3751,#2142,.T.);
#4575=EDGE_CURVE('',#3753,#3752,#2793,.T.);
#4576=EDGE_CURVE('',#3750,#3753,#2143,.T.);
#4577=EDGE_CURVE('',#3754,#3755,#2794,.T.);
#4578=EDGE_CURVE('',#3756,#3754,#2795,.T.);
#4579=EDGE_CURVE('',#3757,#3756,#2796,.T.);
#4580=EDGE_CURVE('',#3755,#3757,#2797,.T.);
#4581=EDGE_CURVE('',#3758,#3759,#2144,.T.);
#4582=EDGE_CURVE('',#3759,#3760,#2798,.T.);
#4583=EDGE_CURVE('',#3760,#3761,#2145,.T.);
#4584=EDGE_CURVE('',#3761,#3758,#2799,.T.);
#4585=EDGE_CURVE('',#3762,#3763,#2146,.T.);
#4586=EDGE_CURVE('',#3763,#3764,#2800,.T.);
#4587=EDGE_CURVE('',#3764,#3765,#2147,.T.);
#4588=EDGE_CURVE('',#3765,#3762,#2801,.T.);
#4589=EDGE_CURVE('',#3766,#3767,#2148,.T.);
#4590=EDGE_CURVE('',#3767,#3768,#2802,.T.);
#4591=EDGE_CURVE('',#3768,#3769,#2149,.T.);
#4592=EDGE_CURVE('',#3769,#3766,#2803,.T.);
#4593=EDGE_CURVE('',#3746,#3750,#2804,.T.);
#4594=EDGE_CURVE('',#3753,#3748,#2805,.T.);
#4595=EDGE_CURVE('',#3749,#3752,#2806,.T.);
#4596=EDGE_CURVE('',#3751,#3747,#2807,.T.);
#4597=EDGE_CURVE('',#3759,#3770,#2808,.T.);
#4598=EDGE_CURVE('',#3758,#3771,#2809,.T.);
#4599=EDGE_CURVE('',#3770,#3771,#2150,.T.);
#4600=EDGE_CURVE('',#3760,#3772,#2810,.T.);
#4601=EDGE_CURVE('',#3773,#3772,#2151,.T.);
#4602=EDGE_CURVE('',#3761,#3773,#2811,.T.);
#4603=EDGE_CURVE('',#3771,#3773,#2812,.T.);
#4604=EDGE_CURVE('',#3772,#3770,#2813,.T.);
#4605=EDGE_CURVE('',#3774,#3775,#2814,.T.);
#4606=EDGE_CURVE('',#3776,#3774,#2152,.T.);
#4607=EDGE_CURVE('',#3767,#3776,#2815,.T.);
#4608=EDGE_CURVE('',#3766,#3777,#2816,.T.);
#4609=EDGE_CURVE('',#3778,#3777,#2153,.T.);
#4610=EDGE_CURVE('',#3779,#3778,#2817,.T.);
#4611=EDGE_CURVE('',#3775,#3779,#2154,.T.);
#4612=EDGE_CURVE('',#3768,#3780,#2818,.T.);
#4613=EDGE_CURVE('',#3781,#3780,#2155,.T.);
#4614=EDGE_CURVE('',#3769,#3781,#2819,.T.);
#4615=EDGE_CURVE('',#3777,#3781,#2820,.T.);
#4616=EDGE_CURVE('',#3780,#3776,#2821,.T.);
#4617=EDGE_CURVE('',#3782,#3783,#2822,.T.);
#4618=EDGE_CURVE('',#3784,#3782,#2156,.T.);
#4619=EDGE_CURVE('',#3763,#3784,#2823,.T.);
#4620=EDGE_CURVE('',#3762,#3785,#2824,.T.);
#4621=EDGE_CURVE('',#3786,#3785,#2157,.T.);
#4622=EDGE_CURVE('',#3787,#3786,#2825,.T.);
#4623=EDGE_CURVE('',#3783,#3787,#2158,.T.);
#4624=EDGE_CURVE('',#3764,#3788,#2826,.T.);
#4625=EDGE_CURVE('',#3789,#3788,#2159,.T.);
#4626=EDGE_CURVE('',#3765,#3789,#2827,.T.);
#4627=EDGE_CURVE('',#3785,#3789,#2828,.T.);
#4628=EDGE_CURVE('',#3788,#3784,#2829,.T.);
#4629=EDGE_CURVE('',#3782,#3786,#2160,.T.);
#4630=EDGE_CURVE('',#3787,#3783,#2161,.T.);
#4631=EDGE_CURVE('',#3790,#3790,#2162,.T.);
#4632=EDGE_CURVE('',#3790,#3791,#2830,.T.);
#4633=EDGE_CURVE('',#3791,#3791,#2163,.T.);
#4634=EDGE_CURVE('',#3792,#3792,#2164,.T.);
#4635=EDGE_CURVE('',#3792,#3793,#2831,.T.);
#4636=EDGE_CURVE('',#3793,#3793,#2165,.T.);
#4637=EDGE_CURVE('',#3774,#3778,#2166,.T.);
#4638=EDGE_CURVE('',#3779,#3775,#2167,.T.);
#4639=EDGE_CURVE('',#3754,#3794,#2832,.T.);
#4640=EDGE_CURVE('',#3795,#3794,#2833,.T.);
#4641=EDGE_CURVE('',#3756,#3795,#2834,.T.);
#4642=EDGE_CURVE('',#3796,#3795,#2835,.T.);
#4643=EDGE_CURVE('',#3757,#3796,#2836,.T.);
#4644=EDGE_CURVE('',#3797,#3796,#2837,.T.);
#4645=EDGE_CURVE('',#3755,#3797,#2838,.T.);
#4646=EDGE_CURVE('',#3794,#3797,#2839,.T.);
#4647=EDGE_CURVE('',#3798,#3799,#2840,.T.);
#4648=EDGE_CURVE('',#3799,#3800,#2841,.T.);
#4649=EDGE_CURVE('',#3801,#3800,#2842,.T.);
#4650=EDGE_CURVE('',#3798,#3801,#2843,.T.);
#4651=EDGE_CURVE('',#3802,#3798,#2844,.T.);
#4652=EDGE_CURVE('',#3803,#3801,#2845,.T.);
#4653=EDGE_CURVE('',#3802,#3803,#2846,.T.);
#4654=EDGE_CURVE('',#3804,#3802,#2847,.T.);
#4655=EDGE_CURVE('',#3805,#3803,#2848,.T.);
#4656=EDGE_CURVE('',#3804,#3805,#2849,.T.);
#4657=EDGE_CURVE('',#3799,#3804,#2850,.T.);
#4658=EDGE_CURVE('',#3800,#3805,#2851,.T.);
#4659=EDGE_CURVE('',#3806,#3807,#2852,.T.);
#4660=EDGE_CURVE('',#3807,#3808,#2853,.T.);
#4661=EDGE_CURVE('',#3809,#3808,#2854,.T.);
#4662=EDGE_CURVE('',#3806,#3809,#2855,.T.);
#4663=EDGE_CURVE('',#3810,#3806,#2856,.T.);
#4664=EDGE_CURVE('',#3811,#3809,#2857,.T.);
#4665=EDGE_CURVE('',#3810,#3811,#2858,.T.);
#4666=EDGE_CURVE('',#3812,#3810,#2859,.T.);
#4667=EDGE_CURVE('',#3813,#3811,#2860,.T.);
#4668=EDGE_CURVE('',#3812,#3813,#2861,.T.);
#4669=EDGE_CURVE('',#3807,#3812,#2862,.T.);
#4670=EDGE_CURVE('',#3808,#3813,#2863,.T.);
#4671=EDGE_CURVE('',#3814,#3814,#2168,.T.);
#4672=EDGE_CURVE('',#3814,#3815,#2864,.T.);
#4673=EDGE_CURVE('',#3815,#3815,#2169,.T.);
#4674=EDGE_CURVE('',#3816,#3816,#2170,.T.);
#4675=EDGE_CURVE('',#3816,#3817,#2865,.T.);
#4676=EDGE_CURVE('',#3817,#3817,#2171,.T.);
#4677=EDGE_CURVE('',#3818,#3818,#2172,.T.);
#4678=EDGE_CURVE('',#3818,#3819,#2866,.T.);
#4679=EDGE_CURVE('',#3819,#3819,#2173,.T.);
#4680=EDGE_CURVE('',#3820,#3820,#2174,.T.);
#4681=EDGE_CURVE('',#3820,#3821,#2867,.T.);
#4682=EDGE_CURVE('',#3821,#3821,#2175,.T.);
#4683=EDGE_CURVE('',#3822,#3822,#2176,.T.);
#4684=EDGE_CURVE('',#3822,#3823,#2868,.T.);
#4685=EDGE_CURVE('',#3823,#3823,#2177,.T.);
#4686=EDGE_CURVE('',#3824,#3824,#2178,.T.);
#4687=EDGE_CURVE('',#3824,#3825,#2869,.T.);
#4688=EDGE_CURVE('',#3825,#3825,#2179,.T.);
#4689=EDGE_CURVE('',#3826,#3826,#2180,.T.);
#4690=EDGE_CURVE('',#3826,#3827,#2870,.T.);
#4691=EDGE_CURVE('',#3827,#3827,#2181,.T.);
#4692=EDGE_CURVE('',#3828,#3828,#2182,.T.);
#4693=EDGE_CURVE('',#3828,#3829,#2871,.T.);
#4694=EDGE_CURVE('',#3829,#3829,#2183,.T.);
#4695=EDGE_CURVE('',#3830,#3830,#2184,.T.);
#4696=EDGE_CURVE('',#3830,#3831,#2872,.T.);
#4697=EDGE_CURVE('',#3831,#3831,#2185,.T.);
#4698=EDGE_CURVE('',#3832,#3833,#2873,.T.);
#4699=EDGE_CURVE('',#3834,#3832,#2874,.T.);
#4700=EDGE_CURVE('',#3834,#3835,#2875,.T.);
#4701=EDGE_CURVE('',#3833,#3835,#2876,.T.);
#4702=EDGE_CURVE('',#3836,#3837,#2877,.T.);
#4703=EDGE_CURVE('',#3838,#3836,#2878,.T.);
#4704=EDGE_CURVE('',#3839,#3838,#2879,.T.);
#4705=EDGE_CURVE('',#3837,#3839,#2880,.T.);
#4706=EDGE_CURVE('',#3839,#3840,#2881,.T.);
#4707=EDGE_CURVE('',#3841,#3838,#2882,.T.);
#4708=EDGE_CURVE('',#3840,#3841,#2883,.T.);
#4709=EDGE_CURVE('',#3842,#3834,#2884,.T.);
#4710=EDGE_CURVE('',#3842,#3843,#2885,.T.);
#4711=EDGE_CURVE('',#3835,#3843,#2886,.T.);
#4712=EDGE_CURVE('',#3832,#3844,#2887,.T.);
#4713=EDGE_CURVE('',#3845,#3844,#2888,.T.);
#4714=EDGE_CURVE('',#3837,#3845,#2889,.T.);
#4715=EDGE_CURVE('',#3840,#3842,#2890,.T.);
#4716=EDGE_CURVE('',#3833,#3846,#2891,.T.);
#4717=EDGE_CURVE('',#3844,#3846,#2892,.T.);
#4718=EDGE_CURVE('',#3836,#3847,#2893,.T.);
#4719=EDGE_CURVE('',#3846,#3847,#2894,.T.);
#4720=EDGE_CURVE('',#3843,#3841,#2895,.T.);
#4721=EDGE_CURVE('',#3847,#3845,#2896,.T.);
#4722=EDGE_CURVE('',#3848,#3848,#2186,.T.);
#4723=EDGE_CURVE('',#3848,#3849,#2897,.T.);
#4724=EDGE_CURVE('',#3849,#3849,#2187,.T.);
#4725=EDGE_CURVE('',#3850,#3850,#2188,.T.);
#4726=EDGE_CURVE('',#3850,#3851,#2898,.T.);
#4727=EDGE_CURVE('',#3851,#3851,#2189,.T.);
#4728=EDGE_CURVE('',#3852,#3853,#2899,.T.);
#4729=EDGE_CURVE('',#3854,#3852,#2190,.T.);
#4730=EDGE_CURVE('',#3855,#3854,#2900,.T.);
#4731=EDGE_CURVE('',#3853,#3855,#2191,.T.);
#4732=EDGE_CURVE('',#3856,#3857,#2901,.T.);
#4733=EDGE_CURVE('',#3858,#3856,#2192,.T.);
#4734=EDGE_CURVE('',#3859,#3858,#2902,.T.);
#4735=EDGE_CURVE('',#3857,#3859,#2193,.T.);
#4736=EDGE_CURVE('',#3860,#3861,#2903,.T.);
#4737=EDGE_CURVE('',#3862,#3860,#2194,.T.);
#4738=EDGE_CURVE('',#3863,#3862,#2904,.T.);
#4739=EDGE_CURVE('',#3861,#3863,#2195,.T.);
#4740=EDGE_CURVE('',#3864,#3865,#2905,.T.);
#4741=EDGE_CURVE('',#3866,#3864,#2196,.T.);
#4742=EDGE_CURVE('',#3867,#3866,#2906,.T.);
#4743=EDGE_CURVE('',#3865,#3867,#2197,.T.);
#4744=EDGE_CURVE('',#3866,#3852,#2198,.T.);
#4745=EDGE_CURVE('',#3862,#3864,#2199,.T.);
#4746=EDGE_CURVE('',#3858,#3860,#2200,.T.);
#4747=EDGE_CURVE('',#3854,#3856,#2201,.T.);
#4748=EDGE_CURVE('',#3868,#3868,#2202,.T.);
#4749=EDGE_CURVE('',#3863,#3865,#2203,.T.);
#4750=EDGE_CURVE('',#3859,#3861,#2204,.T.);
#4751=EDGE_CURVE('',#3867,#3853,#2205,.T.);
#4752=EDGE_CURVE('',#3855,#3857,#2206,.T.);
#4753=EDGE_CURVE('',#3869,#3869,#2207,.T.);
#4754=EDGE_CURVE('',#3869,#3870,#2907,.T.);
#4755=EDGE_CURVE('',#3870,#3870,#2208,.T.);
#4756=EDGE_CURVE('',#3871,#3871,#2209,.T.);
#4757=EDGE_CURVE('',#3871,#3868,#2908,.T.);
#4758=EDGE_CURVE('',#3872,#3873,#2909,.T.);
#4759=EDGE_CURVE('',#3874,#3872,#2210,.T.);
#4760=EDGE_CURVE('',#3875,#3874,#2910,.T.);
#4761=EDGE_CURVE('',#3873,#3875,#2211,.T.);
#4762=EDGE_CURVE('',#3876,#3877,#2911,.T.);
#4763=EDGE_CURVE('',#3878,#3876,#2212,.T.);
#4764=EDGE_CURVE('',#3879,#3878,#2912,.T.);
#4765=EDGE_CURVE('',#3877,#3879,#2213,.T.);
#4766=EDGE_CURVE('',#3880,#3881,#2913,.T.);
#4767=EDGE_CURVE('',#3882,#3880,#2214,.T.);
#4768=EDGE_CURVE('',#3883,#3882,#2914,.T.);
#4769=EDGE_CURVE('',#3881,#3883,#2215,.T.);
#4770=EDGE_CURVE('',#3884,#3885,#2915,.T.);
#4771=EDGE_CURVE('',#3886,#3884,#2216,.T.);
#4772=EDGE_CURVE('',#3887,#3886,#2916,.T.);
#4773=EDGE_CURVE('',#3885,#3887,#2217,.T.);
#4774=EDGE_CURVE('',#3886,#3872,#2218,.T.);
#4775=EDGE_CURVE('',#3882,#3884,#2219,.T.);
#4776=EDGE_CURVE('',#3878,#3880,#2220,.T.);
#4777=EDGE_CURVE('',#3874,#3876,#2221,.T.);
#4778=EDGE_CURVE('',#3888,#3888,#2222,.T.);
#4779=EDGE_CURVE('',#3883,#3885,#2223,.T.);
#4780=EDGE_CURVE('',#3879,#3881,#2224,.T.);
#4781=EDGE_CURVE('',#3887,#3873,#2225,.T.);
#4782=EDGE_CURVE('',#3875,#3877,#2226,.T.);
#4783=EDGE_CURVE('',#3888,#3889,#2917,.T.);
#4784=EDGE_CURVE('',#3889,#3889,#2227,.T.);
#4785=EDGE_CURVE('',#3890,#3890,#2228,.T.);
#4786=EDGE_CURVE('',#3891,#3891,#2229,.T.);
#4787=EDGE_CURVE('',#3891,#3890,#2918,.T.);
#4788=EDGE_CURVE('',#3892,#3892,#2230,.T.);
#4789=EDGE_CURVE('',#3892,#3893,#2919,.T.);
#4790=EDGE_CURVE('',#3893,#3893,#2231,.T.);
#4791=EDGE_CURVE('',#3894,#3894,#2232,.T.);
#4792=EDGE_CURVE('',#3894,#3895,#2920,.T.);
#4793=EDGE_CURVE('',#3895,#3895,#2233,.T.);
#4794=EDGE_CURVE('',#3896,#3896,#2234,.T.);
#4795=EDGE_CURVE('',#3896,#3897,#2921,.T.);
#4796=EDGE_CURVE('',#3897,#3897,#2235,.T.);
#4797=EDGE_CURVE('',#3898,#3898,#2236,.T.);
#4798=EDGE_CURVE('',#3898,#3899,#2922,.T.);
#4799=EDGE_CURVE('',#3899,#3899,#2237,.T.);
#4800=EDGE_CURVE('',#3900,#3900,#2238,.T.);
#4801=EDGE_CURVE('',#3900,#3901,#2923,.T.);
#4802=EDGE_CURVE('',#3901,#3901,#2239,.T.);
#4803=EDGE_CURVE('',#3902,#3902,#2240,.T.);
#4804=EDGE_CURVE('',#3902,#3903,#2924,.T.);
#4805=EDGE_CURVE('',#3903,#3903,#2241,.T.);
#4806=EDGE_CURVE('',#3904,#3904,#2242,.T.);
#4807=EDGE_CURVE('',#3904,#3905,#2925,.T.);
#4808=EDGE_CURVE('',#3905,#3905,#2243,.T.);
#4809=EDGE_CURVE('',#3906,#3906,#2244,.T.);
#4810=EDGE_CURVE('',#3906,#3907,#2926,.T.);
#4811=EDGE_CURVE('',#3907,#3907,#2245,.T.);
#4812=EDGE_CURVE('',#3908,#3908,#2246,.T.);
#4813=EDGE_CURVE('',#3908,#3909,#2927,.T.);
#4814=EDGE_CURVE('',#3909,#3909,#2247,.T.);
#4815=EDGE_CURVE('',#3910,#3911,#2928,.T.);
#4816=EDGE_CURVE('',#3912,#3910,#2929,.T.);
#4817=EDGE_CURVE('',#3912,#3913,#2930,.T.);
#4818=EDGE_CURVE('',#3911,#3913,#2931,.T.);
#4819=EDGE_CURVE('',#3914,#3915,#2932,.T.);
#4820=EDGE_CURVE('',#3916,#3914,#2933,.T.);
#4821=EDGE_CURVE('',#3917,#3916,#2934,.T.);
#4822=EDGE_CURVE('',#3915,#3917,#2935,.T.);
#4823=EDGE_CURVE('',#3917,#3918,#2936,.T.);
#4824=EDGE_CURVE('',#3919,#3916,#2937,.T.);
#4825=EDGE_CURVE('',#3918,#3919,#2938,.T.);
#4826=EDGE_CURVE('',#3920,#3912,#2939,.T.);
#4827=EDGE_CURVE('',#3920,#3921,#2940,.T.);
#4828=EDGE_CURVE('',#3913,#3921,#2941,.T.);
#4829=EDGE_CURVE('',#3910,#3922,#2942,.T.);
#4830=EDGE_CURVE('',#3923,#3922,#2943,.T.);
#4831=EDGE_CURVE('',#3915,#3923,#2944,.T.);
#4832=EDGE_CURVE('',#3918,#3920,#2945,.T.);
#4833=EDGE_CURVE('',#3911,#3924,#2946,.T.);
#4834=EDGE_CURVE('',#3922,#3924,#2947,.T.);
#4835=EDGE_CURVE('',#3914,#3925,#2948,.T.);
#4836=EDGE_CURVE('',#3924,#3925,#2949,.T.);
#4837=EDGE_CURVE('',#3921,#3919,#2950,.T.);
#4838=EDGE_CURVE('',#3925,#3923,#2951,.T.);
#4839=EDGE_CURVE('',#3926,#3926,#2248,.T.);
#4840=EDGE_CURVE('',#3926,#3927,#2952,.T.);
#4841=EDGE_CURVE('',#3927,#3927,#2249,.T.);
#4842=EDGE_CURVE('',#3928,#3928,#2250,.T.);
#4843=EDGE_CURVE('',#3928,#3929,#2953,.T.);
#4844=EDGE_CURVE('',#3929,#3929,#2251,.T.);
#4845=EDGE_CURVE('',#3930,#3930,#2252,.T.);
#4846=EDGE_CURVE('',#3930,#3931,#2954,.T.);
#4847=EDGE_CURVE('',#3931,#3931,#2253,.T.);
#4848=EDGE_CURVE('',#3932,#3932,#2254,.T.);
#4849=EDGE_CURVE('',#3932,#3933,#2955,.T.);
#4850=EDGE_CURVE('',#3933,#3933,#2255,.T.);
#4851=EDGE_CURVE('',#3934,#3934,#2256,.T.);
#4852=EDGE_CURVE('',#3934,#3935,#2956,.T.);
#4853=EDGE_CURVE('',#3935,#3935,#2257,.T.);
#4854=EDGE_CURVE('',#3936,#3936,#2258,.T.);
#4855=EDGE_CURVE('',#3936,#3937,#2957,.T.);
#4856=EDGE_CURVE('',#3937,#3937,#2259,.T.);
#4857=EDGE_CURVE('',#3938,#3938,#2260,.T.);
#4858=EDGE_CURVE('',#3938,#3939,#2958,.T.);
#4859=EDGE_CURVE('',#3939,#3939,#2261,.T.);
#4860=EDGE_CURVE('',#3940,#3940,#2262,.T.);
#4861=EDGE_CURVE('',#3940,#3941,#2959,.T.);
#4862=EDGE_CURVE('',#3941,#3941,#2263,.T.);
#4863=EDGE_CURVE('',#3942,#3942,#2264,.T.);
#4864=EDGE_CURVE('',#3942,#3943,#2960,.T.);
#4865=EDGE_CURVE('',#3943,#3943,#2265,.T.);
#4866=EDGE_CURVE('',#3944,#3944,#2266,.T.);
#4867=EDGE_CURVE('',#3944,#3945,#2961,.T.);
#4868=EDGE_CURVE('',#3945,#3945,#2267,.T.);
#4869=EDGE_CURVE('',#3946,#3947,#2962,.T.);
#4870=EDGE_CURVE('',#3948,#3946,#2268,.T.);
#4871=EDGE_CURVE('',#3949,#3948,#2963,.T.);
#4872=EDGE_CURVE('',#3947,#3949,#2269,.T.);
#4873=EDGE_CURVE('',#3950,#3951,#2964,.T.);
#4874=EDGE_CURVE('',#3952,#3950,#2270,.T.);
#4875=EDGE_CURVE('',#3953,#3952,#2965,.T.);
#4876=EDGE_CURVE('',#3951,#3953,#2271,.T.);
#4877=EDGE_CURVE('',#3954,#3955,#2966,.T.);
#4878=EDGE_CURVE('',#3956,#3954,#2272,.T.);
#4879=EDGE_CURVE('',#3957,#3956,#2967,.T.);
#4880=EDGE_CURVE('',#3955,#3957,#2273,.T.);
#4881=EDGE_CURVE('',#3958,#3959,#2968,.T.);
#4882=EDGE_CURVE('',#3960,#3958,#2274,.T.);
#4883=EDGE_CURVE('',#3961,#3960,#2969,.T.);
#4884=EDGE_CURVE('',#3959,#3961,#2275,.T.);
#4885=EDGE_CURVE('',#3960,#3946,#2276,.T.);
#4886=EDGE_CURVE('',#3956,#3958,#2277,.T.);
#4887=EDGE_CURVE('',#3952,#3954,#2278,.T.);
#4888=EDGE_CURVE('',#3948,#3950,#2279,.T.);
#4889=EDGE_CURVE('',#3962,#3962,#2280,.T.);
#4890=EDGE_CURVE('',#3957,#3959,#2281,.T.);
#4891=EDGE_CURVE('',#3953,#3955,#2282,.T.);
#4892=EDGE_CURVE('',#3961,#3947,#2283,.T.);
#4893=EDGE_CURVE('',#3949,#3951,#2284,.T.);
#4894=EDGE_CURVE('',#3963,#3963,#2285,.T.);
#4895=EDGE_CURVE('',#3963,#3964,#2970,.T.);
#4896=EDGE_CURVE('',#3964,#3964,#2286,.T.);
#4897=EDGE_CURVE('',#3965,#3965,#2287,.T.);
#4898=EDGE_CURVE('',#3965,#3962,#2971,.T.);
#4899=EDGE_CURVE('',#3966,#3967,#2972,.T.);
#4900=EDGE_CURVE('',#3968,#3966,#2288,.T.);
#4901=EDGE_CURVE('',#3969,#3968,#2973,.T.);
#4902=EDGE_CURVE('',#3967,#3969,#2289,.T.);
#4903=EDGE_CURVE('',#3970,#3971,#2974,.T.);
#4904=EDGE_CURVE('',#3972,#3970,#2290,.T.);
#4905=EDGE_CURVE('',#3973,#3972,#2975,.T.);
#4906=EDGE_CURVE('',#3971,#3973,#2291,.T.);
#4907=EDGE_CURVE('',#3974,#3975,#2976,.T.);
#4908=EDGE_CURVE('',#3976,#3974,#2292,.T.);
#4909=EDGE_CURVE('',#3977,#3976,#2977,.T.);
#4910=EDGE_CURVE('',#3975,#3977,#2293,.T.);
#4911=EDGE_CURVE('',#3978,#3979,#2978,.T.);
#4912=EDGE_CURVE('',#3980,#3978,#2294,.T.);
#4913=EDGE_CURVE('',#3981,#3980,#2979,.T.);
#4914=EDGE_CURVE('',#3979,#3981,#2295,.T.);
#4915=EDGE_CURVE('',#3980,#3966,#2296,.T.);
#4916=EDGE_CURVE('',#3976,#3978,#2297,.T.);
#4917=EDGE_CURVE('',#3972,#3974,#2298,.T.);
#4918=EDGE_CURVE('',#3968,#3970,#2299,.T.);
#4919=EDGE_CURVE('',#3982,#3982,#2300,.T.);
#4920=EDGE_CURVE('',#3977,#3979,#2301,.T.);
#4921=EDGE_CURVE('',#3973,#3975,#2302,.T.);
#4922=EDGE_CURVE('',#3981,#3967,#2303,.T.);
#4923=EDGE_CURVE('',#3969,#3971,#2304,.T.);
#4924=EDGE_CURVE('',#3982,#3983,#2980,.T.);
#4925=EDGE_CURVE('',#3983,#3983,#2305,.T.);
#4926=EDGE_CURVE('',#3984,#3984,#2306,.T.);
#4927=EDGE_CURVE('',#3985,#3985,#2307,.T.);
#4928=EDGE_CURVE('',#3985,#3984,#2981,.T.);
#4929=EDGE_CURVE('',#3986,#3987,#2982,.T.);
#4930=EDGE_CURVE('',#3988,#3986,#2983,.T.);
#4931=EDGE_CURVE('',#3989,#3988,#2984,.T.);
#4932=EDGE_CURVE('',#3989,#3987,#2985,.T.);
#4933=EDGE_CURVE('',#3990,#3991,#2986,.T.);
#4934=EDGE_CURVE('',#3992,#3990,#2987,.T.);
#4935=EDGE_CURVE('',#3993,#3992,#2988,.T.);
#4936=EDGE_CURVE('',#3991,#3993,#2989,.T.);
#4937=EDGE_CURVE('',#3994,#3995,#2990,.T.);
#4938=EDGE_CURVE('',#3996,#3994,#2308,.T.);
#4939=EDGE_CURVE('',#3997,#3996,#2991,.T.);
#4940=EDGE_CURVE('',#3995,#3997,#2309,.T.);
#4941=EDGE_CURVE('',#3987,#3990,#2310,.T.);
#4942=EDGE_CURVE('',#3991,#3986,#2311,.T.);
#4943=EDGE_CURVE('',#3992,#3989,#2312,.T.);
#4944=EDGE_CURVE('',#3988,#3993,#2313,.T.);
#4945=EDGE_CURVE('',#3997,#3998,#2992,.T.);
#4946=EDGE_CURVE('',#3999,#3998,#2314,.T.);
#4947=EDGE_CURVE('',#3995,#3999,#2993,.T.);
#4948=EDGE_CURVE('',#3996,#4000,#2994,.T.);
#4949=EDGE_CURVE('',#3998,#4000,#2995,.T.);
#4950=EDGE_CURVE('',#4001,#3999,#2996,.T.);
#4951=EDGE_CURVE('',#3994,#4001,#2997,.T.);
#4952=EDGE_CURVE('',#4000,#4001,#2315,.T.);
#4953=EDGE_CURVE('',#4002,#4003,#2316,.T.);
#4954=EDGE_CURVE('',#4003,#4002,#2317,.T.);
#4955=EDGE_CURVE('',#4003,#4004,#2318,.T.);
#4956=EDGE_CURVE('',#4005,#4004,#2319,.T.);
#4957=EDGE_CURVE('',#4004,#4005,#2320,.T.);
#4958=EDGE_CURVE('',#4005,#4006,#2998,.T.);
#4959=EDGE_CURVE('',#4006,#4006,#2321,.T.);
#4960=EDGE_CURVE('',#4007,#4007,#2322,.T.);
#4961=EDGE_CURVE('',#4007,#4008,#2999,.T.);
#4962=EDGE_CURVE('',#4008,#4008,#2323,.T.);
#4963=EDGE_CURVE('',#4008,#4009,#3000,.T.);
#4964=EDGE_CURVE('',#4009,#4009,#2324,.T.);
#4965=EDGE_CURVE('',#4010,#4010,#2325,.T.);
#4966=EDGE_CURVE('',#4010,#4002,#3001,.T.);
#4967=EDGE_CURVE('',#4011,#4011,#2326,.T.);
#4968=EDGE_CURVE('',#4011,#4007,#3002,.T.);
#4969=EDGE_CURVE('',#4012,#4013,#2327,.T.);
#4970=EDGE_CURVE('',#4013,#4012,#2328,.T.);
#4971=EDGE_CURVE('',#4013,#4014,#2329,.T.);
#4972=EDGE_CURVE('',#4015,#4014,#2330,.T.);
#4973=EDGE_CURVE('',#4014,#4015,#2331,.T.);
#4974=EDGE_CURVE('',#4016,#4016,#2332,.T.);
#4975=EDGE_CURVE('',#4016,#4015,#3003,.T.);
#4976=EDGE_CURVE('',#4017,#4017,#2333,.T.);
#4977=EDGE_CURVE('',#4018,#4018,#2334,.T.);
#4978=EDGE_CURVE('',#4019,#4019,#2335,.T.);
#4979=EDGE_CURVE('',#4019,#4017,#3004,.T.);
#4980=EDGE_CURVE('',#4020,#4020,#2336,.T.);
#4981=EDGE_CURVE('',#4020,#4019,#3005,.T.);
#4982=EDGE_CURVE('',#4021,#4021,#2337,.T.);
#4983=EDGE_CURVE('',#4021,#4020,#3006,.T.);
#4984=EDGE_CURVE('',#4012,#4018,#3007,.T.);
#4985=EDGE_CURVE('',#4022,#4023,#2338,.T.);
#4986=EDGE_CURVE('',#4024,#4025,#2339,.T.);
#4987=EDGE_CURVE('',#4026,#4027,#2340,.T.);
#4988=EDGE_CURVE('',#4028,#4029,#2341,.T.);
#4989=EDGE_CURVE('',#4030,#4031,#2342,.T.);
#4990=EDGE_CURVE('',#4032,#4033,#2343,.T.);
#4991=EDGE_CURVE('',#4034,#4035,#2344,.T.);
#4992=EDGE_CURVE('',#4036,#4037,#2345,.T.);
#4993=EDGE_CURVE('',#4038,#4039,#309,.T.);
#4994=EDGE_CURVE('',#4040,#4038,#2346,.T.);
#4995=EDGE_CURVE('',#4041,#4040,#310,.T.);
#4996=EDGE_CURVE('',#4039,#4041,#2347,.T.);
#4997=EDGE_CURVE('',#4042,#4040,#2348,.T.);
#4998=EDGE_CURVE('',#4042,#4043,#311,.T.);
#4999=EDGE_CURVE('',#4044,#4043,#2349,.T.);
#5000=EDGE_CURVE('',#4044,#4045,#312,.T.);
#5001=EDGE_CURVE('',#4046,#4045,#2350,.T.);
#5002=EDGE_CURVE('',#4046,#4047,#313,.T.);
#5003=EDGE_CURVE('',#4047,#4048,#3008,.T.);
#5004=EDGE_CURVE('',#4048,#4048,#2351,.T.);
#5005=EDGE_CURVE('',#4047,#4049,#314,.T.);
#5006=EDGE_CURVE('',#4050,#4049,#2352,.T.);
#5007=EDGE_CURVE('',#4050,#4051,#315,.T.);
#5008=EDGE_CURVE('',#4052,#4051,#2353,.T.);
#5009=EDGE_CURVE('',#4052,#4053,#316,.T.);
#5010=EDGE_CURVE('',#4054,#4053,#2354,.T.);
#5011=EDGE_CURVE('',#4054,#4055,#317,.T.);
#5012=EDGE_CURVE('',#4056,#4055,#2355,.T.);
#5013=EDGE_CURVE('',#4056,#4057,#318,.T.);
#5014=EDGE_CURVE('',#4041,#4057,#2356,.T.);
#5015=EDGE_CURVE('',#4038,#4058,#2357,.T.);
#5016=EDGE_CURVE('',#4058,#4042,#2358,.T.);
#5017=EDGE_CURVE('',#4059,#4058,#319,.T.);
#5018=EDGE_CURVE('',#4043,#4059,#2359,.T.);
#5019=EDGE_CURVE('',#4059,#4060,#2360,.T.);
#5020=EDGE_CURVE('',#4060,#4044,#2361,.T.);
#5021=EDGE_CURVE('',#4061,#4060,#320,.T.);
#5022=EDGE_CURVE('',#4045,#4061,#2362,.T.);
#5023=EDGE_CURVE('',#4061,#4062,#2363,.T.);
#5024=EDGE_CURVE('',#4062,#4046,#2364,.T.);
#5025=EDGE_CURVE('',#4063,#4064,#321,.T.);
#5026=EDGE_CURVE('',#4049,#4063,#2365,.T.);
#5027=EDGE_CURVE('',#4064,#4062,#322,.T.);
#5028=EDGE_CURVE('',#4063,#4065,#2366,.T.);
#5029=EDGE_CURVE('',#4065,#4050,#2367,.T.);
#5030=EDGE_CURVE('',#4066,#4065,#323,.T.);
#5031=EDGE_CURVE('',#4051,#4066,#2368,.T.);
#5032=EDGE_CURVE('',#4066,#4067,#2369,.T.);
#5033=EDGE_CURVE('',#4067,#4052,#2370,.T.);
#5034=EDGE_CURVE('',#4068,#4067,#324,.T.);
#5035=EDGE_CURVE('',#4053,#4068,#2371,.T.);
#5036=EDGE_CURVE('',#4068,#4069,#2372,.T.);
#5037=EDGE_CURVE('',#4069,#4054,#2373,.T.);
#5038=EDGE_CURVE('',#4070,#4069,#325,.T.);
#5039=EDGE_CURVE('',#4055,#4070,#2374,.T.);
#5040=EDGE_CURVE('',#4071,#4071,#2375,.T.);
#5041=EDGE_CURVE('',#4071,#4064,#3009,.T.);
#5042=EDGE_CURVE('',#4072,#4039,#2376,.T.);
#5043=EDGE_CURVE('',#4072,#4073,#326,.T.);
#5044=EDGE_CURVE('',#4070,#4073,#2377,.T.);
#5045=EDGE_CURVE('',#4057,#4072,#2378,.T.);
#5046=EDGE_CURVE('',#4073,#4056,#2379,.T.);
#5047=EDGE_CURVE('',#4074,#4074,#2380,.T.);
#5048=EDGE_CURVE('',#4075,#4075,#2381,.T.);
#5049=EDGE_CURVE('',#4076,#4076,#2382,.T.);
#5050=EDGE_CURVE('',#4076,#4074,#3010,.T.);
#5051=EDGE_CURVE('',#4077,#4077,#2383,.T.);
#5052=EDGE_CURVE('',#4077,#4075,#3011,.T.);
#5053=EDGE_CURVE('',#4078,#4078,#2384,.T.);
#5054=EDGE_CURVE('',#4079,#4079,#2385,.T.);
#5055=EDGE_CURVE('',#4080,#4080,#2386,.T.);
#5056=EDGE_CURVE('',#4080,#4078,#3012,.T.);
#5057=EDGE_CURVE('',#4081,#4081,#2387,.T.);
#5058=EDGE_CURVE('',#4081,#4079,#3013,.T.);
#5059=EDGE_CURVE('',#4082,#4083,#3014,.T.);
#5060=EDGE_CURVE('',#4083,#4084,#3015,.T.);
#5061=EDGE_CURVE('',#4084,#4085,#3016,.T.);
#5062=EDGE_CURVE('',#4082,#4085,#3017,.T.);
#5063=EDGE_CURVE('',#4083,#4086,#3018,.T.);
#5064=EDGE_CURVE('',#4086,#4087,#3019,.T.);
#5065=EDGE_CURVE('',#4087,#4084,#3020,.T.);
#5066=EDGE_CURVE('',#4086,#4088,#3021,.T.);
#5067=EDGE_CURVE('',#4088,#4089,#3022,.T.);
#5068=EDGE_CURVE('',#4089,#4087,#3023,.T.);
#5069=EDGE_CURVE('',#4088,#4090,#3024,.T.);
#5070=EDGE_CURVE('',#4090,#4091,#3025,.T.);
#5071=EDGE_CURVE('',#4091,#4089,#3026,.T.);
#5072=EDGE_CURVE('',#4090,#4092,#3027,.T.);
#5073=EDGE_CURVE('',#4092,#4093,#3028,.T.);
#5074=EDGE_CURVE('',#4093,#4091,#3029,.T.);
#5075=EDGE_CURVE('',#4092,#4082,#3030,.T.);
#5076=EDGE_CURVE('',#4085,#4093,#3031,.T.);
#5077=EDGE_CURVE('',#4094,#4094,#2388,.T.);
#5078=EDGE_CURVE('',#4095,#4095,#2389,.T.);
#5079=EDGE_CURVE('',#4094,#4096,#3032,.T.);
#5080=EDGE_CURVE('',#4096,#4096,#2390,.T.);
#5081=EDGE_CURVE('',#4097,#4097,#2391,.T.);
#5082=EDGE_CURVE('',#4098,#4098,#2392,.T.);
#5083=EDGE_CURVE('',#4098,#4097,#3033,.T.);
#5084=EDGE_CURVE('',#4099,#4099,#2393,.T.);
#5085=EDGE_CURVE('',#4099,#4098,#3034,.T.);
#5086=EDGE_CURVE('',#4100,#4100,#2394,.T.);
#5087=EDGE_CURVE('',#4100,#4099,#3035,.T.);
#5088=EDGE_CURVE('',#4101,#4101,#2395,.T.);
#5089=EDGE_CURVE('',#4102,#4102,#2396,.F.);
#5090=EDGE_CURVE('',#4102,#4101,#3036,.T.);
#5091=EDGE_CURVE('',#4103,#4103,#2397,.F.);
#5092=EDGE_CURVE('',#4103,#4102,#3037,.T.);
#5093=EDGE_CURVE('',#4095,#4103,#3038,.T.);
#5094=EDGE_CURVE('',#4104,#4105,#2398,.T.);
#5095=EDGE_CURVE('',#4105,#4104,#2399,.T.);
#5096=EDGE_CURVE('',#4105,#4106,#2400,.T.);
#5097=EDGE_CURVE('',#4107,#4106,#2401,.T.);
#5098=EDGE_CURVE('',#4106,#4107,#2402,.T.);
#5099=EDGE_CURVE('',#4107,#4108,#3039,.T.);
#5100=EDGE_CURVE('',#4108,#4108,#2403,.T.);
#5101=EDGE_CURVE('',#4109,#4109,#2404,.T.);
#5102=EDGE_CURVE('',#4109,#4110,#3040,.T.);
#5103=EDGE_CURVE('',#4110,#4110,#2405,.T.);
#5104=EDGE_CURVE('',#4110,#4111,#3041,.T.);
#5105=EDGE_CURVE('',#4111,#4111,#2406,.T.);
#5106=EDGE_CURVE('',#4112,#4112,#2407,.T.);
#5107=EDGE_CURVE('',#4112,#4104,#3042,.T.);
#5108=EDGE_CURVE('',#4113,#4113,#2408,.T.);
#5109=EDGE_CURVE('',#4113,#4109,#3043,.T.);
#5110=EDGE_CURVE('',#4114,#4115,#2409,.T.);
#5111=EDGE_CURVE('',#4115,#4114,#2410,.T.);
#5112=EDGE_CURVE('',#4115,#4116,#2411,.T.);
#5113=EDGE_CURVE('',#4117,#4116,#2412,.T.);
#5114=EDGE_CURVE('',#4116,#4117,#2413,.T.);
#5115=EDGE_CURVE('',#4118,#4118,#2414,.T.);
#5116=EDGE_CURVE('',#4118,#4117,#3044,.T.);
#5117=EDGE_CURVE('',#4119,#4119,#2415,.T.);
#5118=EDGE_CURVE('',#4120,#4120,#2416,.T.);
#5119=EDGE_CURVE('',#4121,#4121,#2417,.T.);
#5120=EDGE_CURVE('',#4121,#4119,#3045,.T.);
#5121=EDGE_CURVE('',#4122,#4122,#2418,.T.);
#5122=EDGE_CURVE('',#4122,#4121,#3046,.T.);
#5123=EDGE_CURVE('',#4123,#4123,#2419,.T.);
#5124=EDGE_CURVE('',#4123,#4122,#3047,.T.);
#5125=EDGE_CURVE('',#4114,#4120,#3048,.T.);
#5126=EDGE_CURVE('',#4124,#4125,#2420,.T.);
#5127=EDGE_CURVE('',#4126,#4127,#2421,.T.);
#5128=EDGE_CURVE('',#4128,#4129,#2422,.T.);
#5129=EDGE_CURVE('',#4130,#4131,#2423,.T.);
#5130=EDGE_CURVE('',#4132,#4133,#2424,.T.);
#5131=EDGE_CURVE('',#4134,#4135,#2425,.T.);
#5132=EDGE_CURVE('',#4136,#4137,#2426,.T.);
#5133=EDGE_CURVE('',#4138,#4139,#327,.T.);
#5134=EDGE_CURVE('',#4140,#4138,#2427,.T.);
#5135=EDGE_CURVE('',#4141,#4140,#328,.T.);
#5136=EDGE_CURVE('',#4139,#4141,#2428,.T.);
#5137=EDGE_CURVE('',#4142,#4140,#2429,.T.);
#5138=EDGE_CURVE('',#4142,#4143,#329,.T.);
#5139=EDGE_CURVE('',#4144,#4143,#2430,.T.);
#5140=EDGE_CURVE('',#4144,#4145,#330,.T.);
#5141=EDGE_CURVE('',#4146,#4145,#2431,.T.);
#5142=EDGE_CURVE('',#4146,#4147,#3049,.T.);
#5143=EDGE_CURVE('',#4147,#4147,#2432,.T.);
#5144=EDGE_CURVE('',#4148,#4146,#2433,.T.);
#5145=EDGE_CURVE('',#4148,#4149,#331,.T.);
#5146=EDGE_CURVE('',#4150,#4149,#2434,.T.);
#5147=EDGE_CURVE('',#4150,#4151,#332,.T.);
#5148=EDGE_CURVE('',#4152,#4151,#2435,.T.);
#5149=EDGE_CURVE('',#4152,#4153,#333,.T.);
#5150=EDGE_CURVE('',#4154,#4153,#2436,.T.);
#5151=EDGE_CURVE('',#4154,#4155,#334,.T.);
#5152=EDGE_CURVE('',#4141,#4155,#2437,.T.);
#5153=EDGE_CURVE('',#4138,#4156,#2438,.T.);
#5154=EDGE_CURVE('',#4156,#4142,#2439,.T.);
#5155=EDGE_CURVE('',#4157,#4156,#335,.T.);
#5156=EDGE_CURVE('',#4143,#4157,#2440,.T.);
#5157=EDGE_CURVE('',#4157,#4158,#2441,.T.);
#5158=EDGE_CURVE('',#4158,#4144,#2442,.T.);
#5159=EDGE_CURVE('',#4159,#4158,#336,.T.);
#5160=EDGE_CURVE('',#4145,#4159,#2443,.T.);
#5161=EDGE_CURVE('',#4159,#4160,#2444,.T.);
#5162=EDGE_CURVE('',#4160,#4161,#2445,.T.);
#5163=EDGE_CURVE('',#4161,#4148,#2446,.T.);
#5164=EDGE_CURVE('',#4162,#4161,#337,.T.);
#5165=EDGE_CURVE('',#4149,#4162,#2447,.T.);
#5166=EDGE_CURVE('',#4162,#4163,#2448,.T.);
#5167=EDGE_CURVE('',#4163,#4150,#2449,.T.);
#5168=EDGE_CURVE('',#4164,#4163,#338,.T.);
#5169=EDGE_CURVE('',#4151,#4164,#2450,.T.);
#5170=EDGE_CURVE('',#4164,#4165,#2451,.T.);
#5171=EDGE_CURVE('',#4165,#4152,#2452,.T.);
#5172=EDGE_CURVE('',#4166,#4165,#339,.T.);
#5173=EDGE_CURVE('',#4153,#4166,#2453,.T.);
#5174=EDGE_CURVE('',#4167,#4167,#2454,.T.);
#5175=EDGE_CURVE('',#4167,#4160,#3050,.T.);
#5176=EDGE_CURVE('',#4168,#4139,#2455,.T.);
#5177=EDGE_CURVE('',#4168,#4169,#340,.T.);
#5178=EDGE_CURVE('',#4166,#4169,#2456,.T.);
#5179=EDGE_CURVE('',#4155,#4168,#2457,.T.);
#5180=EDGE_CURVE('',#4169,#4154,#2458,.T.);
#5181=EDGE_CURVE('',#4170,#4170,#2459,.T.);
#5182=EDGE_CURVE('',#4171,#4171,#2460,.T.);
#5183=EDGE_CURVE('',#4172,#4172,#2461,.T.);
#5184=EDGE_CURVE('',#4172,#4170,#3051,.T.);
#5185=EDGE_CURVE('',#4173,#4173,#2462,.T.);
#5186=EDGE_CURVE('',#4173,#4171,#3052,.T.);
#5187=EDGE_CURVE('',#4174,#4174,#2463,.T.);
#5188=EDGE_CURVE('',#4175,#4175,#2464,.T.);
#5189=EDGE_CURVE('',#4176,#4176,#2465,.T.);
#5190=EDGE_CURVE('',#4176,#4174,#3053,.T.);
#5191=EDGE_CURVE('',#4177,#4177,#2466,.T.);
#5192=EDGE_CURVE('',#4177,#4175,#3054,.T.);
#5193=EDGE_CURVE('',#4178,#4179,#3055,.T.);
#5194=EDGE_CURVE('',#4179,#4180,#3056,.T.);
#5195=EDGE_CURVE('',#4180,#4181,#3057,.T.);
#5196=EDGE_CURVE('',#4178,#4181,#3058,.T.);
#5197=EDGE_CURVE('',#4179,#4182,#3059,.T.);
#5198=EDGE_CURVE('',#4182,#4183,#3060,.T.);
#5199=EDGE_CURVE('',#4183,#4180,#3061,.T.);
#5200=EDGE_CURVE('',#4182,#4184,#3062,.T.);
#5201=EDGE_CURVE('',#4184,#4185,#3063,.T.);
#5202=EDGE_CURVE('',#4185,#4183,#3064,.T.);
#5203=EDGE_CURVE('',#4184,#4186,#3065,.T.);
#5204=EDGE_CURVE('',#4186,#4187,#3066,.T.);
#5205=EDGE_CURVE('',#4187,#4185,#3067,.T.);
#5206=EDGE_CURVE('',#4186,#4188,#3068,.T.);
#5207=EDGE_CURVE('',#4188,#4189,#3069,.T.);
#5208=EDGE_CURVE('',#4189,#4187,#3070,.T.);
#5209=EDGE_CURVE('',#4188,#4178,#3071,.T.);
#5210=EDGE_CURVE('',#4181,#4189,#3072,.T.);
#5211=EDGE_CURVE('',#4190,#4190,#2467,.T.);
#5212=EDGE_CURVE('',#4191,#4191,#2468,.T.);
#5213=EDGE_CURVE('',#4192,#4192,#2469,.T.);
#5214=EDGE_CURVE('',#4192,#4191,#3073,.T.);
#5215=EDGE_CURVE('',#4193,#4193,#2470,.T.);
#5216=EDGE_CURVE('',#4193,#4192,#3074,.T.);
#5217=EDGE_CURVE('',#4194,#4194,#2471,.T.);
#5218=EDGE_CURVE('',#4194,#4193,#3075,.T.);
#5219=EDGE_CURVE('',#4195,#4195,#2472,.T.);
#5220=EDGE_CURVE('',#4196,#4196,#2473,.F.);
#5221=EDGE_CURVE('',#4196,#4195,#3076,.T.);
#5222=EDGE_CURVE('',#4190,#4196,#3077,.T.);
#5223=EDGE_CURVE('',#4197,#4197,#2474,.T.);
#5224=EDGE_CURVE('',#4197,#4198,#3078,.T.);
#5225=EDGE_CURVE('',#4198,#4198,#2475,.T.);
#5226=EDGE_CURVE('',#4199,#4199,#2476,.T.);
#5227=EDGE_CURVE('',#4200,#4200,#2477,.T.);
#5228=EDGE_CURVE('',#4201,#4201,#2478,.T.);
#5229=EDGE_CURVE('',#4202,#4202,#2479,.T.);
#5230=EDGE_CURVE('',#4199,#4201,#3079,.T.);
#5231=EDGE_CURVE('',#4202,#4203,#3080,.T.);
#5232=EDGE_CURVE('',#4203,#4203,#2480,.T.);
#5233=EDGE_CURVE('',#4204,#4204,#2481,.T.);
#5234=EDGE_CURVE('',#4204,#4205,#3081,.T.);
#5235=EDGE_CURVE('',#4205,#4205,#2482,.T.);
#5236=EDGE_CURVE('',#4206,#4206,#2483,.T.);
#5237=EDGE_CURVE('',#4206,#4200,#3082,.T.);
#5238=EDGE_CURVE('',#4207,#4207,#2484,.T.);
#5239=EDGE_CURVE('',#4207,#4208,#3083,.T.);
#5240=EDGE_CURVE('',#4208,#4208,#2485,.T.);
#5241=EDGE_CURVE('',#4209,#4209,#2486,.T.);
#5242=EDGE_CURVE('',#4209,#4210,#3084,.T.);
#5243=EDGE_CURVE('',#4210,#4210,#2487,.T.);
#5244=EDGE_CURVE('',#4211,#4211,#2488,.T.);
#5245=EDGE_CURVE('',#4211,#4212,#3085,.T.);
#5246=EDGE_CURVE('',#4212,#4212,#2489,.T.);
#5247=EDGE_CURVE('',#4213,#4213,#2490,.T.);
#5248=EDGE_CURVE('',#4213,#4214,#3086,.T.);
#5249=EDGE_CURVE('',#4214,#4214,#2491,.T.);
#5250=EDGE_CURVE('',#4215,#4215,#2492,.T.);
#5251=EDGE_CURVE('',#4215,#4216,#3087,.T.);
#5252=EDGE_CURVE('',#4216,#4216,#2493,.T.);
#5253=EDGE_CURVE('',#4217,#4217,#2494,.T.);
#5254=EDGE_CURVE('',#4217,#4218,#3088,.T.);
#5255=EDGE_CURVE('',#4218,#4218,#2495,.T.);
#5256=EDGE_CURVE('',#4219,#4219,#2496,.T.);
#5257=EDGE_CURVE('',#4219,#4220,#3089,.T.);
#5258=EDGE_CURVE('',#4220,#4220,#2497,.T.);
#5259=EDGE_CURVE('',#4221,#4221,#2498,.T.);
#5260=EDGE_CURVE('',#4221,#4222,#3090,.T.);
#5261=EDGE_CURVE('',#4222,#4222,#2499,.T.);
#5262=EDGE_CURVE('',#4223,#4223,#2500,.T.);
#5263=EDGE_CURVE('',#4223,#4224,#3091,.T.);
#5264=EDGE_CURVE('',#4224,#4224,#2501,.T.);
#5265=EDGE_CURVE('',#4225,#4226,#341,.T.);
#5266=EDGE_CURVE('',#4227,#4225,#342,.T.);
#5267=EDGE_CURVE('',#4226,#4227,#343,.T.);
#5268=EDGE_CURVE('',#4226,#4228,#3092,.T.);
#5269=EDGE_CURVE('',#4229,#4228,#344,.T.);
#5270=EDGE_CURVE('',#4230,#4229,#345,.T.);
#5271=EDGE_CURVE('',#4231,#4230,#346,.T.);
#5272=EDGE_CURVE('',#4228,#4231,#347,.T.);
#5273=EDGE_CURVE('',#4232,#4233,#348,.T.);
#5274=EDGE_CURVE('',#4233,#4232,#349,.T.);
#5275=EDGE_CURVE('',#4233,#4234,#3093,.T.);
#5276=EDGE_CURVE('',#4235,#4234,#350,.T.);
#5277=EDGE_CURVE('',#4236,#4235,#351,.T.);
#5278=EDGE_CURVE('',#4234,#4236,#352,.T.);
#5279=EDGE_CURVE('',#4237,#4237,#2502,.T.);
#5280=EDGE_CURVE('',#4237,#4227,#3094,.T.);
#5281=EDGE_CURVE('',#4225,#4238,#3095,.T.);
#5282=EDGE_CURVE('',#4238,#4238,#2503,.T.);
#5283=EDGE_CURVE('',#4239,#4240,#353,.T.);
#5284=EDGE_CURVE('',#4240,#4241,#354,.T.);
#5285=EDGE_CURVE('',#4241,#4239,#355,.T.);
#5286=EDGE_CURVE('',#4242,#4243,#356,.T.);
#5287=EDGE_CURVE('',#4243,#4244,#357,.T.);
#5288=EDGE_CURVE('',#4244,#4242,#358,.T.);
#5289=EDGE_CURVE('',#4241,#4245,#3096,.T.);
#5290=EDGE_CURVE('',#4246,#4245,#359,.T.);
#5291=EDGE_CURVE('',#4245,#4246,#360,.T.);
#5292=EDGE_CURVE('',#4247,#4248,#361,.T.);
#5293=EDGE_CURVE('',#4248,#4247,#362,.T.);
#5294=EDGE_CURVE('',#4248,#4244,#3097,.T.);
#5295=EDGE_CURVE('',#4249,#4249,#2504,.T.);
#5296=EDGE_CURVE('',#4249,#4229,#3098,.T.);
#5297=EDGE_CURVE('',#4231,#4250,#3099,.T.);
#5298=EDGE_CURVE('',#4250,#4250,#2505,.T.);
#5299=EDGE_CURVE('',#4251,#4251,#2506,.T.);
#5300=EDGE_CURVE('',#4252,#4253,#2507,.T.);
#5301=EDGE_CURVE('',#4254,#4253,#2508,.T.);
#5302=EDGE_CURVE('',#4254,#4255,#2509,.T.);
#5303=EDGE_CURVE('',#4256,#4255,#2510,.T.);
#5304=EDGE_CURVE('',#4256,#4257,#2511,.T.);
#5305=EDGE_CURVE('',#4258,#4257,#2512,.T.);
#5306=EDGE_CURVE('',#4258,#4259,#2513,.T.);
#5307=EDGE_CURVE('',#4260,#4259,#2514,.T.);
#5308=EDGE_CURVE('',#4260,#4261,#2515,.T.);
#5309=EDGE_CURVE('',#4262,#4261,#2516,.T.);
#5310=EDGE_CURVE('',#4262,#4263,#2517,.T.);
#5311=EDGE_CURVE('',#4264,#4263,#2518,.T.);
#5312=EDGE_CURVE('',#4264,#4265,#2519,.T.);
#5313=EDGE_CURVE('',#4266,#4265,#2520,.T.);
#5314=EDGE_CURVE('',#4266,#4267,#2521,.T.);
#5315=EDGE_CURVE('',#4268,#4267,#2522,.T.);
#5316=EDGE_CURVE('',#4268,#4269,#2523,.T.);
#5317=EDGE_CURVE('',#4270,#4269,#2524,.T.);
#5318=EDGE_CURVE('',#4270,#4271,#2525,.T.);
#5319=EDGE_CURVE('',#4272,#4271,#2526,.T.);
#5320=EDGE_CURVE('',#4272,#4273,#2527,.T.);
#5321=EDGE_CURVE('',#4274,#4273,#2528,.T.);
#5322=EDGE_CURVE('',#4274,#4275,#2529,.T.);
#5323=EDGE_CURVE('',#4276,#4275,#2530,.T.);
#5324=EDGE_CURVE('',#4276,#4277,#2531,.T.);
#5325=EDGE_CURVE('',#4278,#4277,#2532,.T.);
#5326=EDGE_CURVE('',#4278,#4279,#2533,.T.);
#5327=EDGE_CURVE('',#4280,#4279,#2534,.T.);
#5328=EDGE_CURVE('',#4280,#4281,#2535,.T.);
#5329=EDGE_CURVE('',#4282,#4281,#2536,.T.);
#5330=EDGE_CURVE('',#4282,#4283,#2537,.T.);
#5331=EDGE_CURVE('',#4284,#4283,#2538,.T.);
#5332=EDGE_CURVE('',#4284,#4285,#2539,.T.);
#5333=EDGE_CURVE('',#4286,#4285,#2540,.T.);
#5334=EDGE_CURVE('',#4286,#4287,#2541,.T.);
#5335=EDGE_CURVE('',#4288,#4287,#2542,.T.);
#5336=EDGE_CURVE('',#4288,#4289,#2543,.T.);
#5337=EDGE_CURVE('',#4290,#4289,#2544,.T.);
#5338=EDGE_CURVE('',#4290,#4291,#2545,.T.);
#5339=EDGE_CURVE('',#4252,#4291,#2546,.T.);
#5340=EDGE_CURVE('',#4292,#4292,#2547,.T.);
#5341=EDGE_CURVE('',#4292,#4251,#3100,.T.);
#5342=EDGE_CURVE('',#4293,#4293,#2548,.T.);
#5343=EDGE_CURVE('',#4294,#4295,#2549,.T.);
#5344=EDGE_CURVE('',#4295,#4296,#2550,.T.);
#5345=EDGE_CURVE('',#4296,#4297,#2551,.T.);
#5346=EDGE_CURVE('',#4297,#4298,#2552,.T.);
#5347=EDGE_CURVE('',#4298,#4299,#2553,.T.);
#5348=EDGE_CURVE('',#4299,#4300,#2554,.T.);
#5349=EDGE_CURVE('',#4300,#4301,#2555,.T.);
#5350=EDGE_CURVE('',#4301,#4302,#2556,.T.);
#5351=EDGE_CURVE('',#4302,#4303,#2557,.T.);
#5352=EDGE_CURVE('',#4303,#4304,#2558,.T.);
#5353=EDGE_CURVE('',#4304,#4305,#2559,.T.);
#5354=EDGE_CURVE('',#4305,#4306,#2560,.T.);
#5355=EDGE_CURVE('',#4306,#4307,#2561,.T.);
#5356=EDGE_CURVE('',#4307,#4308,#2562,.T.);
#5357=EDGE_CURVE('',#4308,#4309,#2563,.T.);
#5358=EDGE_CURVE('',#4309,#4310,#2564,.T.);
#5359=EDGE_CURVE('',#4310,#4311,#2565,.T.);
#5360=EDGE_CURVE('',#4311,#4312,#2566,.T.);
#5361=EDGE_CURVE('',#4312,#4313,#2567,.T.);
#5362=EDGE_CURVE('',#4313,#4314,#2568,.T.);
#5363=EDGE_CURVE('',#4314,#4315,#2569,.T.);
#5364=EDGE_CURVE('',#4315,#4316,#2570,.T.);
#5365=EDGE_CURVE('',#4316,#4317,#2571,.T.);
#5366=EDGE_CURVE('',#4317,#4318,#2572,.T.);
#5367=EDGE_CURVE('',#4318,#4319,#2573,.T.);
#5368=EDGE_CURVE('',#4319,#4320,#2574,.T.);
#5369=EDGE_CURVE('',#4320,#4321,#2575,.T.);
#5370=EDGE_CURVE('',#4321,#4322,#2576,.T.);
#5371=EDGE_CURVE('',#4322,#4323,#2577,.T.);
#5372=EDGE_CURVE('',#4323,#4324,#2578,.T.);
#5373=EDGE_CURVE('',#4324,#4325,#2579,.T.);
#5374=EDGE_CURVE('',#4325,#4326,#2580,.T.);
#5375=EDGE_CURVE('',#4326,#4327,#2581,.T.);
#5376=EDGE_CURVE('',#4327,#4328,#2582,.T.);
#5377=EDGE_CURVE('',#4328,#4329,#2583,.T.);
#5378=EDGE_CURVE('',#4329,#4330,#2584,.T.);
#5379=EDGE_CURVE('',#4330,#4331,#2585,.T.);
#5380=EDGE_CURVE('',#4331,#4332,#2586,.T.);
#5381=EDGE_CURVE('',#4332,#4333,#2587,.T.);
#5382=EDGE_CURVE('',#4333,#4294,#2588,.T.);
#5383=EDGE_CURVE('',#4334,#4334,#2589,.T.);
#5384=EDGE_CURVE('',#4334,#4293,#3101,.T.);
#5385=EDGE_CURVE('',#4295,#4252,#3102,.T.);
#5386=EDGE_CURVE('',#4253,#4294,#3103,.T.);
#5387=EDGE_CURVE('',#4333,#4254,#3104,.T.);
#5388=EDGE_CURVE('',#4255,#4332,#3105,.T.);
#5389=EDGE_CURVE('',#4331,#4256,#3106,.T.);
#5390=EDGE_CURVE('',#4257,#4330,#3107,.T.);
#5391=EDGE_CURVE('',#4329,#4258,#3108,.T.);
#5392=EDGE_CURVE('',#4259,#4328,#3109,.T.);
#5393=EDGE_CURVE('',#4327,#4260,#3110,.T.);
#5394=EDGE_CURVE('',#4261,#4326,#3111,.T.);
#5395=EDGE_CURVE('',#4325,#4262,#3112,.T.);
#5396=EDGE_CURVE('',#4263,#4324,#3113,.T.);
#5397=EDGE_CURVE('',#4323,#4264,#3114,.T.);
#5398=EDGE_CURVE('',#4265,#4322,#3115,.T.);
#5399=EDGE_CURVE('',#4321,#4266,#3116,.T.);
#5400=EDGE_CURVE('',#4267,#4320,#3117,.T.);
#5401=EDGE_CURVE('',#4319,#4268,#3118,.T.);
#5402=EDGE_CURVE('',#4269,#4318,#3119,.T.);
#5403=EDGE_CURVE('',#4317,#4270,#3120,.T.);
#5404=EDGE_CURVE('',#4271,#4316,#3121,.T.);
#5405=EDGE_CURVE('',#4315,#4272,#3122,.T.);
#5406=EDGE_CURVE('',#4273,#4314,#3123,.T.);
#5407=EDGE_CURVE('',#4313,#4274,#3124,.T.);
#5408=EDGE_CURVE('',#4275,#4312,#3125,.T.);
#5409=EDGE_CURVE('',#4311,#4276,#3126,.T.);
#5410=EDGE_CURVE('',#4277,#4310,#3127,.T.);
#5411=EDGE_CURVE('',#4309,#4278,#3128,.T.);
#5412=EDGE_CURVE('',#4279,#4308,#3129,.T.);
#5413=EDGE_CURVE('',#4307,#4280,#3130,.T.);
#5414=EDGE_CURVE('',#4281,#4306,#3131,.T.);
#5415=EDGE_CURVE('',#4305,#4282,#3132,.T.);
#5416=EDGE_CURVE('',#4283,#4304,#3133,.T.);
#5417=EDGE_CURVE('',#4303,#4284,#3134,.T.);
#5418=EDGE_CURVE('',#4285,#4302,#3135,.T.);
#5419=EDGE_CURVE('',#4301,#4286,#3136,.T.);
#5420=EDGE_CURVE('',#4287,#4300,#3137,.T.);
#5421=EDGE_CURVE('',#4299,#4288,#3138,.T.);
#5422=EDGE_CURVE('',#4289,#4298,#3139,.T.);
#5423=EDGE_CURVE('',#4291,#4296,#3140,.T.);
#5424=EDGE_CURVE('',#4297,#4290,#3141,.T.);
#5425=EDGE_CURVE('',#4335,#4335,#2590,.T.);
#5426=EDGE_CURVE('',#4335,#4336,#3142,.T.);
#5427=EDGE_CURVE('',#4336,#4336,#2591,.T.);
#5428=EDGE_CURVE('',#4337,#4337,#2592,.T.);
#5429=EDGE_CURVE('',#4338,#4338,#2593,.T.);
#5430=EDGE_CURVE('',#4339,#4339,#2594,.T.);
#5431=EDGE_CURVE('',#4340,#4340,#2595,.T.);
#5432=EDGE_CURVE('',#4337,#4339,#3143,.T.);
#5433=EDGE_CURVE('',#4340,#4341,#3144,.T.);
#5434=EDGE_CURVE('',#4341,#4341,#2596,.T.);
#5435=EDGE_CURVE('',#4342,#4342,#2597,.T.);
#5436=EDGE_CURVE('',#4342,#4338,#3145,.T.);
#5437=EDGE_CURVE('',#4343,#4343,#2598,.T.);
#5438=EDGE_CURVE('',#4343,#4344,#3146,.T.);
#5439=EDGE_CURVE('',#4344,#4344,#2599,.T.);
#5440=EDGE_CURVE('',#4345,#4345,#2600,.T.);
#5441=EDGE_CURVE('',#4345,#4346,#3147,.T.);
#5442=EDGE_CURVE('',#4346,#4346,#2601,.T.);
#5443=EDGE_CURVE('',#4347,#4347,#2602,.T.);
#5444=EDGE_CURVE('',#4347,#4348,#3148,.T.);
#5445=EDGE_CURVE('',#4348,#4348,#2603,.T.);
#5446=EDGE_CURVE('',#4349,#4349,#2604,.T.);
#5447=EDGE_CURVE('',#4349,#4350,#3149,.T.);
#5448=EDGE_CURVE('',#4350,#4350,#2605,.T.);
#5449=EDGE_CURVE('',#4351,#4351,#2606,.T.);
#5450=EDGE_CURVE('',#4351,#4352,#3150,.T.);
#5451=EDGE_CURVE('',#4352,#4352,#2607,.T.);
#5452=EDGE_CURVE('',#4353,#4353,#2608,.T.);
#5453=EDGE_CURVE('',#4353,#4354,#3151,.T.);
#5454=EDGE_CURVE('',#4354,#4354,#2609,.T.);
#5455=EDGE_CURVE('',#4355,#4355,#2610,.T.);
#5456=EDGE_CURVE('',#4355,#4356,#3152,.T.);
#5457=EDGE_CURVE('',#4356,#4356,#2611,.T.);
#5458=EDGE_CURVE('',#4357,#4357,#2612,.T.);
#5459=EDGE_CURVE('',#4357,#4358,#3153,.T.);
#5460=EDGE_CURVE('',#4358,#4358,#2613,.T.);
#5461=EDGE_CURVE('',#4359,#4360,#363,.T.);
#5462=EDGE_CURVE('',#4361,#4359,#364,.T.);
#5463=EDGE_CURVE('',#4360,#4361,#365,.T.);
#5464=EDGE_CURVE('',#4360,#4362,#3154,.T.);
#5465=EDGE_CURVE('',#4363,#4362,#366,.T.);
#5466=EDGE_CURVE('',#4364,#4363,#367,.T.);
#5467=EDGE_CURVE('',#4365,#4364,#368,.T.);
#5468=EDGE_CURVE('',#4362,#4365,#369,.T.);
#5469=EDGE_CURVE('',#4366,#4367,#370,.T.);
#5470=EDGE_CURVE('',#4367,#4366,#371,.T.);
#5471=EDGE_CURVE('',#4367,#4368,#3155,.T.);
#5472=EDGE_CURVE('',#4369,#4368,#372,.T.);
#5473=EDGE_CURVE('',#4370,#4369,#373,.T.);
#5474=EDGE_CURVE('',#4368,#4370,#374,.T.);
#5475=EDGE_CURVE('',#4371,#4371,#2614,.T.);
#5476=EDGE_CURVE('',#4371,#4361,#3156,.T.);
#5477=EDGE_CURVE('',#4359,#4372,#3157,.T.);
#5478=EDGE_CURVE('',#4372,#4372,#2615,.T.);
#5479=EDGE_CURVE('',#4373,#4374,#375,.T.);
#5480=EDGE_CURVE('',#4374,#4375,#376,.T.);
#5481=EDGE_CURVE('',#4375,#4373,#377,.T.);
#5482=EDGE_CURVE('',#4376,#4377,#378,.T.);
#5483=EDGE_CURVE('',#4377,#4378,#379,.T.);
#5484=EDGE_CURVE('',#4378,#4376,#380,.T.);
#5485=EDGE_CURVE('',#4375,#4379,#3158,.T.);
#5486=EDGE_CURVE('',#4380,#4379,#381,.T.);
#5487=EDGE_CURVE('',#4379,#4380,#382,.T.);
#5488=EDGE_CURVE('',#4381,#4382,#383,.T.);
#5489=EDGE_CURVE('',#4382,#4381,#384,.T.);
#5490=EDGE_CURVE('',#4382,#4378,#3159,.T.);
#5491=EDGE_CURVE('',#4383,#4383,#2616,.T.);
#5492=EDGE_CURVE('',#4383,#4363,#3160,.T.);
#5493=EDGE_CURVE('',#4365,#4384,#3161,.T.);
#5494=EDGE_CURVE('',#4384,#4384,#2617,.T.);
#5495=EDGE_CURVE('',#4385,#4385,#2618,.T.);
#5496=EDGE_CURVE('',#4386,#4387,#2619,.T.);
#5497=EDGE_CURVE('',#4388,#4387,#2620,.T.);
#5498=EDGE_CURVE('',#4388,#4389,#2621,.T.);
#5499=EDGE_CURVE('',#4390,#4389,#2622,.T.);
#5500=EDGE_CURVE('',#4390,#4391,#2623,.T.);
#5501=EDGE_CURVE('',#4392,#4391,#2624,.T.);
#5502=EDGE_CURVE('',#4392,#4393,#2625,.T.);
#5503=EDGE_CURVE('',#4394,#4393,#2626,.T.);
#5504=EDGE_CURVE('',#4394,#4395,#2627,.T.);
#5505=EDGE_CURVE('',#4396,#4395,#2628,.T.);
#5506=EDGE_CURVE('',#4396,#4397,#2629,.T.);
#5507=EDGE_CURVE('',#4398,#4397,#2630,.T.);
#5508=EDGE_CURVE('',#4398,#4399,#2631,.T.);
#5509=EDGE_CURVE('',#4400,#4399,#2632,.T.);
#5510=EDGE_CURVE('',#4400,#4401,#2633,.T.);
#5511=EDGE_CURVE('',#4402,#4401,#2634,.T.);
#5512=EDGE_CURVE('',#4402,#4403,#2635,.T.);
#5513=EDGE_CURVE('',#4404,#4403,#2636,.T.);
#5514=EDGE_CURVE('',#4404,#4405,#2637,.T.);
#5515=EDGE_CURVE('',#4406,#4405,#2638,.T.);
#5516=EDGE_CURVE('',#4406,#4407,#2639,.T.);
#5517=EDGE_CURVE('',#4408,#4407,#2640,.T.);
#5518=EDGE_CURVE('',#4408,#4409,#2641,.T.);
#5519=EDGE_CURVE('',#4410,#4409,#2642,.T.);
#5520=EDGE_CURVE('',#4410,#4411,#2643,.T.);
#5521=EDGE_CURVE('',#4412,#4411,#2644,.T.);
#5522=EDGE_CURVE('',#4412,#4413,#2645,.T.);
#5523=EDGE_CURVE('',#4414,#4413,#2646,.T.);
#5524=EDGE_CURVE('',#4414,#4415,#2647,.T.);
#5525=EDGE_CURVE('',#4416,#4415,#2648,.T.);
#5526=EDGE_CURVE('',#4416,#4417,#2649,.T.);
#5527=EDGE_CURVE('',#4418,#4417,#2650,.T.);
#5528=EDGE_CURVE('',#4418,#4419,#2651,.T.);
#5529=EDGE_CURVE('',#4420,#4419,#2652,.T.);
#5530=EDGE_CURVE('',#4420,#4421,#2653,.T.);
#5531=EDGE_CURVE('',#4422,#4421,#2654,.T.);
#5532=EDGE_CURVE('',#4422,#4423,#2655,.T.);
#5533=EDGE_CURVE('',#4424,#4423,#2656,.T.);
#5534=EDGE_CURVE('',#4424,#4425,#2657,.T.);
#5535=EDGE_CURVE('',#4426,#4425,#2658,.T.);
#5536=EDGE_CURVE('',#4426,#4427,#2659,.T.);
#5537=EDGE_CURVE('',#4428,#4427,#2660,.T.);
#5538=EDGE_CURVE('',#4428,#4429,#2661,.T.);
#5539=EDGE_CURVE('',#4430,#4429,#2662,.T.);
#5540=EDGE_CURVE('',#4430,#4431,#2663,.T.);
#5541=EDGE_CURVE('',#4432,#4431,#2664,.T.);
#5542=EDGE_CURVE('',#4432,#4433,#2665,.T.);
#5543=EDGE_CURVE('',#4434,#4433,#2666,.T.);
#5544=EDGE_CURVE('',#4434,#4435,#2667,.T.);
#5545=EDGE_CURVE('',#4436,#4435,#2668,.T.);
#5546=EDGE_CURVE('',#4436,#4437,#2669,.T.);
#5547=EDGE_CURVE('',#4438,#4437,#2670,.T.);
#5548=EDGE_CURVE('',#4438,#4439,#2671,.T.);
#5549=EDGE_CURVE('',#4440,#4439,#2672,.T.);
#5550=EDGE_CURVE('',#4440,#4441,#2673,.T.);
#5551=EDGE_CURVE('',#4442,#4441,#2674,.T.);
#5552=EDGE_CURVE('',#4442,#4443,#2675,.T.);
#5553=EDGE_CURVE('',#4444,#4443,#2676,.T.);
#5554=EDGE_CURVE('',#4444,#4445,#2677,.T.);
#5555=EDGE_CURVE('',#4446,#4445,#2678,.T.);
#5556=EDGE_CURVE('',#4446,#4447,#2679,.T.);
#5557=EDGE_CURVE('',#4448,#4447,#2680,.T.);
#5558=EDGE_CURVE('',#4448,#4449,#2681,.T.);
#5559=EDGE_CURVE('',#4450,#4449,#2682,.T.);
#5560=EDGE_CURVE('',#4450,#4451,#2683,.T.);
#5561=EDGE_CURVE('',#4452,#4451,#2684,.T.);
#5562=EDGE_CURVE('',#4452,#4453,#2685,.T.);
#5563=EDGE_CURVE('',#4454,#4453,#2686,.T.);
#5564=EDGE_CURVE('',#4454,#4455,#2687,.T.);
#5565=EDGE_CURVE('',#4456,#4455,#2688,.T.);
#5566=EDGE_CURVE('',#4456,#4457,#2689,.T.);
#5567=EDGE_CURVE('',#4458,#4457,#2690,.T.);
#5568=EDGE_CURVE('',#4458,#4459,#2691,.T.);
#5569=EDGE_CURVE('',#4460,#4459,#2692,.T.);
#5570=EDGE_CURVE('',#4460,#4461,#2693,.T.);
#5571=EDGE_CURVE('',#4462,#4461,#2694,.T.);
#5572=EDGE_CURVE('',#4462,#4463,#2695,.T.);
#5573=EDGE_CURVE('',#4464,#4463,#2696,.T.);
#5574=EDGE_CURVE('',#4464,#4465,#2697,.T.);
#5575=EDGE_CURVE('',#4386,#4465,#2698,.T.);
#5576=EDGE_CURVE('',#4466,#4466,#2699,.T.);
#5577=EDGE_CURVE('',#4466,#4385,#3162,.T.);
#5578=EDGE_CURVE('',#4467,#4467,#2700,.T.);
#5579=EDGE_CURVE('',#4468,#4469,#2701,.T.);
#5580=EDGE_CURVE('',#4469,#4470,#2702,.T.);
#5581=EDGE_CURVE('',#4470,#4471,#2703,.T.);
#5582=EDGE_CURVE('',#4471,#4472,#2704,.T.);
#5583=EDGE_CURVE('',#4472,#4473,#2705,.T.);
#5584=EDGE_CURVE('',#4473,#4474,#2706,.T.);
#5585=EDGE_CURVE('',#4474,#4475,#2707,.T.);
#5586=EDGE_CURVE('',#4475,#4476,#2708,.T.);
#5587=EDGE_CURVE('',#4476,#4477,#2709,.T.);
#5588=EDGE_CURVE('',#4477,#4478,#2710,.T.);
#5589=EDGE_CURVE('',#4478,#4479,#2711,.T.);
#5590=EDGE_CURVE('',#4479,#4480,#2712,.T.);
#5591=EDGE_CURVE('',#4480,#4481,#2713,.T.);
#5592=EDGE_CURVE('',#4481,#4482,#2714,.T.);
#5593=EDGE_CURVE('',#4482,#4483,#2715,.T.);
#5594=EDGE_CURVE('',#4483,#4484,#2716,.T.);
#5595=EDGE_CURVE('',#4484,#4485,#2717,.T.);
#5596=EDGE_CURVE('',#4485,#4486,#2718,.T.);
#5597=EDGE_CURVE('',#4486,#4487,#2719,.T.);
#5598=EDGE_CURVE('',#4487,#4488,#2720,.T.);
#5599=EDGE_CURVE('',#4488,#4489,#2721,.T.);
#5600=EDGE_CURVE('',#4489,#4490,#2722,.T.);
#5601=EDGE_CURVE('',#4490,#4491,#2723,.T.);
#5602=EDGE_CURVE('',#4491,#4492,#2724,.T.);
#5603=EDGE_CURVE('',#4492,#4493,#2725,.T.);
#5604=EDGE_CURVE('',#4493,#4494,#2726,.T.);
#5605=EDGE_CURVE('',#4494,#4495,#2727,.T.);
#5606=EDGE_CURVE('',#4495,#4496,#2728,.T.);
#5607=EDGE_CURVE('',#4496,#4497,#2729,.T.);
#5608=EDGE_CURVE('',#4497,#4498,#2730,.T.);
#5609=EDGE_CURVE('',#4498,#4499,#2731,.T.);
#5610=EDGE_CURVE('',#4499,#4500,#2732,.T.);
#5611=EDGE_CURVE('',#4500,#4501,#2733,.T.);
#5612=EDGE_CURVE('',#4501,#4502,#2734,.T.);
#5613=EDGE_CURVE('',#4502,#4503,#2735,.T.);
#5614=EDGE_CURVE('',#4503,#4504,#2736,.T.);
#5615=EDGE_CURVE('',#4504,#4505,#2737,.T.);
#5616=EDGE_CURVE('',#4505,#4506,#2738,.T.);
#5617=EDGE_CURVE('',#4506,#4507,#2739,.T.);
#5618=EDGE_CURVE('',#4507,#4508,#2740,.T.);
#5619=EDGE_CURVE('',#4508,#4509,#2741,.T.);
#5620=EDGE_CURVE('',#4509,#4510,#2742,.T.);
#5621=EDGE_CURVE('',#4510,#4511,#2743,.T.);
#5622=EDGE_CURVE('',#4511,#4512,#2744,.T.);
#5623=EDGE_CURVE('',#4512,#4513,#2745,.T.);
#5624=EDGE_CURVE('',#4513,#4514,#2746,.T.);
#5625=EDGE_CURVE('',#4514,#4515,#2747,.T.);
#5626=EDGE_CURVE('',#4515,#4516,#2748,.T.);
#5627=EDGE_CURVE('',#4516,#4517,#2749,.T.);
#5628=EDGE_CURVE('',#4517,#4518,#2750,.T.);
#5629=EDGE_CURVE('',#4518,#4519,#2751,.T.);
#5630=EDGE_CURVE('',#4519,#4520,#2752,.T.);
#5631=EDGE_CURVE('',#4520,#4521,#2753,.T.);
#5632=EDGE_CURVE('',#4521,#4522,#2754,.T.);
#5633=EDGE_CURVE('',#4522,#4523,#2755,.T.);
#5634=EDGE_CURVE('',#4523,#4524,#2756,.T.);
#5635=EDGE_CURVE('',#4524,#4525,#2757,.T.);
#5636=EDGE_CURVE('',#4525,#4526,#2758,.T.);
#5637=EDGE_CURVE('',#4526,#4527,#2759,.T.);
#5638=EDGE_CURVE('',#4527,#4528,#2760,.T.);
#5639=EDGE_CURVE('',#4528,#4529,#2761,.T.);
#5640=EDGE_CURVE('',#4529,#4530,#2762,.T.);
#5641=EDGE_CURVE('',#4530,#4531,#2763,.T.);
#5642=EDGE_CURVE('',#4531,#4532,#2764,.T.);
#5643=EDGE_CURVE('',#4532,#4533,#2765,.T.);
#5644=EDGE_CURVE('',#4533,#4534,#2766,.T.);
#5645=EDGE_CURVE('',#4534,#4535,#2767,.T.);
#5646=EDGE_CURVE('',#4535,#4536,#2768,.T.);
#5647=EDGE_CURVE('',#4536,#4537,#2769,.T.);
#5648=EDGE_CURVE('',#4537,#4538,#2770,.T.);
#5649=EDGE_CURVE('',#4538,#4539,#2771,.T.);
#5650=EDGE_CURVE('',#4539,#4540,#2772,.T.);
#5651=EDGE_CURVE('',#4540,#4541,#2773,.T.);
#5652=EDGE_CURVE('',#4541,#4542,#2774,.T.);
#5653=EDGE_CURVE('',#4542,#4543,#2775,.T.);
#5654=EDGE_CURVE('',#4543,#4544,#2776,.T.);
#5655=EDGE_CURVE('',#4544,#4545,#2777,.T.);
#5656=EDGE_CURVE('',#4545,#4546,#2778,.T.);
#5657=EDGE_CURVE('',#4546,#4547,#2779,.T.);
#5658=EDGE_CURVE('',#4547,#4468,#2780,.T.);
#5659=EDGE_CURVE('',#4548,#4548,#2781,.T.);
#5660=EDGE_CURVE('',#4548,#4467,#3163,.T.);
#5661=EDGE_CURVE('',#4469,#4386,#3164,.T.);
#5662=EDGE_CURVE('',#4387,#4468,#3165,.T.);
#5663=EDGE_CURVE('',#4547,#4388,#3166,.T.);
#5664=EDGE_CURVE('',#4389,#4546,#3167,.T.);
#5665=EDGE_CURVE('',#4545,#4390,#3168,.T.);
#5666=EDGE_CURVE('',#4391,#4544,#3169,.T.);
#5667=EDGE_CURVE('',#4543,#4392,#3170,.T.);
#5668=EDGE_CURVE('',#4393,#4542,#3171,.T.);
#5669=EDGE_CURVE('',#4541,#4394,#3172,.T.);
#5670=EDGE_CURVE('',#4395,#4540,#3173,.T.);
#5671=EDGE_CURVE('',#4539,#4396,#3174,.T.);
#5672=EDGE_CURVE('',#4397,#4538,#3175,.T.);
#5673=EDGE_CURVE('',#4537,#4398,#3176,.T.);
#5674=EDGE_CURVE('',#4399,#4536,#3177,.T.);
#5675=EDGE_CURVE('',#4535,#4400,#3178,.T.);
#5676=EDGE_CURVE('',#4401,#4534,#3179,.T.);
#5677=EDGE_CURVE('',#4533,#4402,#3180,.T.);
#5678=EDGE_CURVE('',#4403,#4532,#3181,.T.);
#5679=EDGE_CURVE('',#4531,#4404,#3182,.T.);
#5680=EDGE_CURVE('',#4405,#4530,#3183,.T.);
#5681=EDGE_CURVE('',#4529,#4406,#3184,.T.);
#5682=EDGE_CURVE('',#4407,#4528,#3185,.T.);
#5683=EDGE_CURVE('',#4527,#4408,#3186,.T.);
#5684=EDGE_CURVE('',#4409,#4526,#3187,.T.);
#5685=EDGE_CURVE('',#4525,#4410,#3188,.T.);
#5686=EDGE_CURVE('',#4411,#4524,#3189,.T.);
#5687=EDGE_CURVE('',#4523,#4412,#3190,.T.);
#5688=EDGE_CURVE('',#4413,#4522,#3191,.T.);
#5689=EDGE_CURVE('',#4521,#4414,#3192,.T.);
#5690=EDGE_CURVE('',#4415,#4520,#3193,.T.);
#5691=EDGE_CURVE('',#4519,#4416,#3194,.T.);
#5692=EDGE_CURVE('',#4417,#4518,#3195,.T.);
#5693=EDGE_CURVE('',#4517,#4418,#3196,.T.);
#5694=EDGE_CURVE('',#4419,#4516,#3197,.T.);
#5695=EDGE_CURVE('',#4515,#4420,#3198,.T.);
#5696=EDGE_CURVE('',#4421,#4514,#3199,.T.);
#5697=EDGE_CURVE('',#4513,#4422,#3200,.T.);
#5698=EDGE_CURVE('',#4423,#4512,#3201,.T.);
#5699=EDGE_CURVE('',#4511,#4424,#3202,.T.);
#5700=EDGE_CURVE('',#4425,#4510,#3203,.T.);
#5701=EDGE_CURVE('',#4509,#4426,#3204,.T.);
#5702=EDGE_CURVE('',#4427,#4508,#3205,.T.);
#5703=EDGE_CURVE('',#4507,#4428,#3206,.T.);
#5704=EDGE_CURVE('',#4429,#4506,#3207,.T.);
#5705=EDGE_CURVE('',#4505,#4430,#3208,.T.);
#5706=EDGE_CURVE('',#4431,#4504,#3209,.T.);
#5707=EDGE_CURVE('',#4503,#4432,#3210,.T.);
#5708=EDGE_CURVE('',#4433,#4502,#3211,.T.);
#5709=EDGE_CURVE('',#4501,#4434,#3212,.T.);
#5710=EDGE_CURVE('',#4435,#4500,#3213,.T.);
#5711=EDGE_CURVE('',#4499,#4436,#3214,.T.);
#5712=EDGE_CURVE('',#4437,#4498,#3215,.T.);
#5713=EDGE_CURVE('',#4497,#4438,#3216,.T.);
#5714=EDGE_CURVE('',#4439,#4496,#3217,.T.);
#5715=EDGE_CURVE('',#4495,#4440,#3218,.T.);
#5716=EDGE_CURVE('',#4441,#4494,#3219,.T.);
#5717=EDGE_CURVE('',#4493,#4442,#3220,.T.);
#5718=EDGE_CURVE('',#4443,#4492,#3221,.T.);
#5719=EDGE_CURVE('',#4491,#4444,#3222,.T.);
#5720=EDGE_CURVE('',#4445,#4490,#3223,.T.);
#5721=EDGE_CURVE('',#4489,#4446,#3224,.T.);
#5722=EDGE_CURVE('',#4447,#4488,#3225,.T.);
#5723=EDGE_CURVE('',#4487,#4448,#3226,.T.);
#5724=EDGE_CURVE('',#4449,#4486,#3227,.T.);
#5725=EDGE_CURVE('',#4485,#4450,#3228,.T.);
#5726=EDGE_CURVE('',#4451,#4484,#3229,.T.);
#5727=EDGE_CURVE('',#4483,#4452,#3230,.T.);
#5728=EDGE_CURVE('',#4453,#4482,#3231,.T.);
#5729=EDGE_CURVE('',#4481,#4454,#3232,.T.);
#5730=EDGE_CURVE('',#4455,#4480,#3233,.T.);
#5731=EDGE_CURVE('',#4479,#4456,#3234,.T.);
#5732=EDGE_CURVE('',#4457,#4478,#3235,.T.);
#5733=EDGE_CURVE('',#4477,#4458,#3236,.T.);
#5734=EDGE_CURVE('',#4459,#4476,#3237,.T.);
#5735=EDGE_CURVE('',#4475,#4460,#3238,.T.);
#5736=EDGE_CURVE('',#4461,#4474,#3239,.T.);
#5737=EDGE_CURVE('',#4473,#4462,#3240,.T.);
#5738=EDGE_CURVE('',#4463,#4472,#3241,.T.);
#5739=EDGE_CURVE('',#4465,#4470,#3242,.T.);
#5740=EDGE_CURVE('',#4471,#4464,#3243,.T.);
#5741=EDGE_CURVE('',#4549,#4549,#2782,.T.);
#5742=EDGE_CURVE('',#4550,#4550,#2783,.T.);
#5743=EDGE_CURVE('',#4550,#4549,#3244,.T.);
#5744=EDGE_CURVE('',#4551,#4551,#2784,.T.);
#5745=EDGE_CURVE('',#4551,#4550,#3245,.T.);
#5746=EDGE_CURVE('',#4552,#4552,#2785,.T.);
#5747=EDGE_CURVE('',#4552,#4551,#3246,.T.);
#5748=EDGE_CURVE('',#4553,#4553,#2786,.T.);
#5749=EDGE_CURVE('',#4554,#4554,#2787,.F.);
#5750=EDGE_CURVE('',#4554,#4553,#3247,.T.);
#5751=EDGE_CURVE('',#4555,#4555,#2788,.F.);
#5752=EDGE_CURVE('',#4555,#4554,#3248,.T.);
#5753=EDGE_CURVE('',#4556,#4556,#2789,.T.);
#5754=EDGE_CURVE('',#4556,#4555,#3249,.T.);
#5755=EDGE_CURVE('',#4557,#4558,#3250,.T.);
#5756=EDGE_CURVE('',#4558,#4559,#3251,.T.);
#5757=EDGE_CURVE('',#4559,#4560,#3252,.T.);
#5758=EDGE_CURVE('',#4557,#4560,#3253,.T.);
#5759=EDGE_CURVE('',#4558,#4561,#3254,.T.);
#5760=EDGE_CURVE('',#4561,#4562,#3255,.T.);
#5761=EDGE_CURVE('',#4562,#4559,#3256,.T.);
#5762=EDGE_CURVE('',#4561,#4563,#3257,.T.);
#5763=EDGE_CURVE('',#4563,#4564,#3258,.T.);
#5764=EDGE_CURVE('',#4564,#4562,#3259,.T.);
#5765=EDGE_CURVE('',#4563,#4565,#3260,.T.);
#5766=EDGE_CURVE('',#4565,#4566,#3261,.T.);
#5767=EDGE_CURVE('',#4566,#4564,#3262,.T.);
#5768=EDGE_CURVE('',#4565,#4567,#3263,.T.);
#5769=EDGE_CURVE('',#4567,#4568,#3264,.T.);
#5770=EDGE_CURVE('',#4568,#4566,#3265,.T.);
#5771=EDGE_CURVE('',#4567,#4557,#3266,.T.);
#5772=EDGE_CURVE('',#4560,#4568,#3267,.T.);
#5773=ORIENTED_EDGE('',*,*,#4569,.F.);
#5774=ORIENTED_EDGE('',*,*,#4570,.F.);
#5775=ORIENTED_EDGE('',*,*,#4571,.T.);
#5776=ORIENTED_EDGE('',*,*,#4572,.F.);
#5777=ORIENTED_EDGE('',*,*,#4573,.T.);
#5778=ORIENTED_EDGE('',*,*,#4574,.F.);
#5779=ORIENTED_EDGE('',*,*,#4575,.F.);
#5780=ORIENTED_EDGE('',*,*,#4576,.F.);
#5781=ORIENTED_EDGE('',*,*,#4577,.F.);
#5782=ORIENTED_EDGE('',*,*,#4578,.F.);
#5783=ORIENTED_EDGE('',*,*,#4579,.F.);
#5784=ORIENTED_EDGE('',*,*,#4580,.F.);
#5785=ORIENTED_EDGE('',*,*,#4581,.T.);
#5786=ORIENTED_EDGE('',*,*,#4582,.T.);
#5787=ORIENTED_EDGE('',*,*,#4583,.T.);
#5788=ORIENTED_EDGE('',*,*,#4584,.T.);
#5789=ORIENTED_EDGE('',*,*,#4585,.T.);
#5790=ORIENTED_EDGE('',*,*,#4586,.T.);
#5791=ORIENTED_EDGE('',*,*,#4587,.T.);
#5792=ORIENTED_EDGE('',*,*,#4588,.T.);
#5793=ORIENTED_EDGE('',*,*,#4589,.T.);
#5794=ORIENTED_EDGE('',*,*,#4590,.T.);
#5795=ORIENTED_EDGE('',*,*,#4591,.T.);
#5796=ORIENTED_EDGE('',*,*,#4592,.T.);
#5797=ORIENTED_EDGE('',*,*,#4570,.T.);
#5798=ORIENTED_EDGE('',*,*,#4593,.T.);
#5799=ORIENTED_EDGE('',*,*,#4576,.T.);
#5800=ORIENTED_EDGE('',*,*,#4594,.T.);
#5801=ORIENTED_EDGE('',*,*,#4595,.F.);
#5802=ORIENTED_EDGE('',*,*,#4571,.F.);
#5803=ORIENTED_EDGE('',*,*,#4594,.F.);
#5804=ORIENTED_EDGE('',*,*,#4575,.T.);
#5805=ORIENTED_EDGE('',*,*,#4593,.F.);
#5806=ORIENTED_EDGE('',*,*,#4569,.T.);
#5807=ORIENTED_EDGE('',*,*,#4596,.F.);
#5808=ORIENTED_EDGE('',*,*,#4573,.F.);
#5809=ORIENTED_EDGE('',*,*,#4597,.F.);
#5810=ORIENTED_EDGE('',*,*,#4581,.F.);
#5811=ORIENTED_EDGE('',*,*,#4598,.T.);
#5812=ORIENTED_EDGE('',*,*,#4599,.F.);
#5813=ORIENTED_EDGE('',*,*,#4600,.T.);
#5814=ORIENTED_EDGE('',*,*,#4601,.F.);
#5815=ORIENTED_EDGE('',*,*,#4602,.F.);
#5816=ORIENTED_EDGE('',*,*,#4583,.F.);
#5817=ORIENTED_EDGE('',*,*,#4603,.F.);
#5818=ORIENTED_EDGE('',*,*,#4598,.F.);
#5819=ORIENTED_EDGE('',*,*,#4584,.F.);
#5820=ORIENTED_EDGE('',*,*,#4602,.T.);
#5821=ORIENTED_EDGE('',*,*,#4582,.F.);
#5822=ORIENTED_EDGE('',*,*,#4597,.T.);
#5823=ORIENTED_EDGE('',*,*,#4604,.F.);
#5824=ORIENTED_EDGE('',*,*,#4600,.F.);
#5825=ORIENTED_EDGE('',*,*,#4605,.F.);
#5826=ORIENTED_EDGE('',*,*,#4606,.F.);
#5827=ORIENTED_EDGE('',*,*,#4607,.F.);
#5828=ORIENTED_EDGE('',*,*,#4589,.F.);
#5829=ORIENTED_EDGE('',*,*,#4608,.T.);
#5830=ORIENTED_EDGE('',*,*,#4609,.F.);
#5831=ORIENTED_EDGE('',*,*,#4610,.F.);
#5832=ORIENTED_EDGE('',*,*,#4611,.F.);
#5833=ORIENTED_EDGE('',*,*,#4612,.T.);
#5834=ORIENTED_EDGE('',*,*,#4613,.F.);
#5835=ORIENTED_EDGE('',*,*,#4614,.F.);
#5836=ORIENTED_EDGE('',*,*,#4591,.F.);
#5837=ORIENTED_EDGE('',*,*,#4615,.F.);
#5838=ORIENTED_EDGE('',*,*,#4608,.F.);
#5839=ORIENTED_EDGE('',*,*,#4592,.F.);
#5840=ORIENTED_EDGE('',*,*,#4614,.T.);
#5841=ORIENTED_EDGE('',*,*,#4590,.F.);
#5842=ORIENTED_EDGE('',*,*,#4607,.T.);
#5843=ORIENTED_EDGE('',*,*,#4616,.F.);
#5844=ORIENTED_EDGE('',*,*,#4612,.F.);
#5845=ORIENTED_EDGE('',*,*,#4617,.F.);
#5846=ORIENTED_EDGE('',*,*,#4618,.F.);
#5847=ORIENTED_EDGE('',*,*,#4619,.F.);
#5848=ORIENTED_EDGE('',*,*,#4585,.F.);
#5849=ORIENTED_EDGE('',*,*,#4620,.T.);
#5850=ORIENTED_EDGE('',*,*,#4621,.F.);
#5851=ORIENTED_EDGE('',*,*,#4622,.F.);
#5852=ORIENTED_EDGE('',*,*,#4623,.F.);
#5853=ORIENTED_EDGE('',*,*,#4624,.T.);
#5854=ORIENTED_EDGE('',*,*,#4625,.F.);
#5855=ORIENTED_EDGE('',*,*,#4626,.F.);
#5856=ORIENTED_EDGE('',*,*,#4587,.F.);
#5857=ORIENTED_EDGE('',*,*,#4627,.F.);
#5858=ORIENTED_EDGE('',*,*,#4620,.F.);
#5859=ORIENTED_EDGE('',*,*,#4588,.F.);
#5860=ORIENTED_EDGE('',*,*,#4626,.T.);
#5861=ORIENTED_EDGE('',*,*,#4586,.F.);
#5862=ORIENTED_EDGE('',*,*,#4619,.T.);
#5863=ORIENTED_EDGE('',*,*,#4628,.F.);
#5864=ORIENTED_EDGE('',*,*,#4624,.F.);
#5865=ORIENTED_EDGE('',*,*,#4622,.T.);
#5866=ORIENTED_EDGE('',*,*,#4629,.F.);
#5867=ORIENTED_EDGE('',*,*,#4617,.T.);
#5868=ORIENTED_EDGE('',*,*,#4630,.F.);
#5869=ORIENTED_EDGE('',*,*,#4623,.T.);
#5870=ORIENTED_EDGE('',*,*,#4630,.T.);
#5871=ORIENTED_EDGE('',*,*,#4631,.F.);
#5872=ORIENTED_EDGE('',*,*,#4632,.T.);
#5873=ORIENTED_EDGE('',*,*,#4633,.F.);
#5874=ORIENTED_EDGE('',*,*,#4632,.F.);
#5875=ORIENTED_EDGE('',*,*,#4631,.T.);
#5876=ORIENTED_EDGE('',*,*,#4634,.F.);
#5877=ORIENTED_EDGE('',*,*,#4635,.T.);
#5878=ORIENTED_EDGE('',*,*,#4636,.F.);
#5879=ORIENTED_EDGE('',*,*,#4635,.F.);
#5880=ORIENTED_EDGE('',*,*,#4634,.T.);
#5881=ORIENTED_EDGE('',*,*,#4610,.T.);
#5882=ORIENTED_EDGE('',*,*,#4637,.F.);
#5883=ORIENTED_EDGE('',*,*,#4605,.T.);
#5884=ORIENTED_EDGE('',*,*,#4638,.F.);
#5885=ORIENTED_EDGE('',*,*,#4611,.T.);
#5886=ORIENTED_EDGE('',*,*,#4638,.T.);
#5887=ORIENTED_EDGE('',*,*,#4578,.T.);
#5888=ORIENTED_EDGE('',*,*,#4639,.T.);
#5889=ORIENTED_EDGE('',*,*,#4640,.F.);
#5890=ORIENTED_EDGE('',*,*,#4641,.F.);
#5891=ORIENTED_EDGE('',*,*,#4579,.T.);
#5892=ORIENTED_EDGE('',*,*,#4641,.T.);
#5893=ORIENTED_EDGE('',*,*,#4642,.F.);
#5894=ORIENTED_EDGE('',*,*,#4643,.F.);
#5895=ORIENTED_EDGE('',*,*,#4580,.T.);
#5896=ORIENTED_EDGE('',*,*,#4643,.T.);
#5897=ORIENTED_EDGE('',*,*,#4644,.F.);
#5898=ORIENTED_EDGE('',*,*,#4645,.F.);
#5899=ORIENTED_EDGE('',*,*,#4577,.T.);
#5900=ORIENTED_EDGE('',*,*,#4645,.T.);
#5901=ORIENTED_EDGE('',*,*,#4646,.F.);
#5902=ORIENTED_EDGE('',*,*,#4639,.F.);
#5903=ORIENTED_EDGE('',*,*,#4646,.T.);
#5904=ORIENTED_EDGE('',*,*,#4644,.T.);
#5905=ORIENTED_EDGE('',*,*,#4642,.T.);
#5906=ORIENTED_EDGE('',*,*,#4640,.T.);
#5907=ORIENTED_EDGE('',*,*,#4572,.T.);
#5908=ORIENTED_EDGE('',*,*,#4595,.T.);
#5909=ORIENTED_EDGE('',*,*,#4574,.T.);
#5910=ORIENTED_EDGE('',*,*,#4596,.T.);
#5911=ORIENTED_EDGE('',*,*,#4599,.T.);
#5912=ORIENTED_EDGE('',*,*,#4603,.T.);
#5913=ORIENTED_EDGE('',*,*,#4601,.T.);
#5914=ORIENTED_EDGE('',*,*,#4604,.T.);
#5915=ORIENTED_EDGE('',*,*,#4609,.T.);
#5916=ORIENTED_EDGE('',*,*,#4615,.T.);
#5917=ORIENTED_EDGE('',*,*,#4613,.T.);
#5918=ORIENTED_EDGE('',*,*,#4616,.T.);
#5919=ORIENTED_EDGE('',*,*,#4606,.T.);
#5920=ORIENTED_EDGE('',*,*,#4637,.T.);
#5921=ORIENTED_EDGE('',*,*,#4621,.T.);
#5922=ORIENTED_EDGE('',*,*,#4627,.T.);
#5923=ORIENTED_EDGE('',*,*,#4625,.T.);
#5924=ORIENTED_EDGE('',*,*,#4628,.T.);
#5925=ORIENTED_EDGE('',*,*,#4618,.T.);
#5926=ORIENTED_EDGE('',*,*,#4629,.T.);
#5927=ORIENTED_EDGE('',*,*,#4633,.T.);
#5928=ORIENTED_EDGE('',*,*,#4636,.T.);
#5929=ORIENTED_EDGE('',*,*,#4647,.T.);
#5930=ORIENTED_EDGE('',*,*,#4648,.T.);
#5931=ORIENTED_EDGE('',*,*,#4649,.F.);
#5932=ORIENTED_EDGE('',*,*,#4650,.F.);
#5933=ORIENTED_EDGE('',*,*,#4651,.T.);
#5934=ORIENTED_EDGE('',*,*,#4650,.T.);
#5935=ORIENTED_EDGE('',*,*,#4652,.F.);
#5936=ORIENTED_EDGE('',*,*,#4653,.F.);
#5937=ORIENTED_EDGE('',*,*,#4654,.T.);
#5938=ORIENTED_EDGE('',*,*,#4653,.T.);
#5939=ORIENTED_EDGE('',*,*,#4655,.F.);
#5940=ORIENTED_EDGE('',*,*,#4656,.F.);
#5941=ORIENTED_EDGE('',*,*,#4657,.T.);
#5942=ORIENTED_EDGE('',*,*,#4656,.T.);
#5943=ORIENTED_EDGE('',*,*,#4658,.F.);
#5944=ORIENTED_EDGE('',*,*,#4648,.F.);
#5945=ORIENTED_EDGE('',*,*,#4658,.T.);
#5946=ORIENTED_EDGE('',*,*,#4655,.T.);
#5947=ORIENTED_EDGE('',*,*,#4652,.T.);
#5948=ORIENTED_EDGE('',*,*,#4649,.T.);
#5949=ORIENTED_EDGE('',*,*,#4657,.F.);
#5950=ORIENTED_EDGE('',*,*,#4647,.F.);
#5951=ORIENTED_EDGE('',*,*,#4651,.F.);
#5952=ORIENTED_EDGE('',*,*,#4654,.F.);
#5953=ORIENTED_EDGE('',*,*,#4659,.T.);
#5954=ORIENTED_EDGE('',*,*,#4660,.T.);
#5955=ORIENTED_EDGE('',*,*,#4661,.F.);
#5956=ORIENTED_EDGE('',*,*,#4662,.F.);
#5957=ORIENTED_EDGE('',*,*,#4663,.T.);
#5958=ORIENTED_EDGE('',*,*,#4662,.T.);
#5959=ORIENTED_EDGE('',*,*,#4664,.F.);
#5960=ORIENTED_EDGE('',*,*,#4665,.F.);
#5961=ORIENTED_EDGE('',*,*,#4666,.T.);
#5962=ORIENTED_EDGE('',*,*,#4665,.T.);
#5963=ORIENTED_EDGE('',*,*,#4667,.F.);
#5964=ORIENTED_EDGE('',*,*,#4668,.F.);
#5965=ORIENTED_EDGE('',*,*,#4669,.T.);
#5966=ORIENTED_EDGE('',*,*,#4668,.T.);
#5967=ORIENTED_EDGE('',*,*,#4670,.F.);
#5968=ORIENTED_EDGE('',*,*,#4660,.F.);
#5969=ORIENTED_EDGE('',*,*,#4670,.T.);
#5970=ORIENTED_EDGE('',*,*,#4667,.T.);
#5971=ORIENTED_EDGE('',*,*,#4664,.T.);
#5972=ORIENTED_EDGE('',*,*,#4661,.T.);
#5973=ORIENTED_EDGE('',*,*,#4669,.F.);
#5974=ORIENTED_EDGE('',*,*,#4659,.F.);
#5975=ORIENTED_EDGE('',*,*,#4663,.F.);
#5976=ORIENTED_EDGE('',*,*,#4666,.F.);
#5977=ORIENTED_EDGE('',*,*,#4671,.F.);
#5978=ORIENTED_EDGE('',*,*,#4672,.T.);
#5979=ORIENTED_EDGE('',*,*,#4673,.F.);
#5980=ORIENTED_EDGE('',*,*,#4672,.F.);
#5981=ORIENTED_EDGE('',*,*,#4674,.F.);
#5982=ORIENTED_EDGE('',*,*,#4675,.T.);
#5983=ORIENTED_EDGE('',*,*,#4676,.F.);
#5984=ORIENTED_EDGE('',*,*,#4675,.F.);
#5985=ORIENTED_EDGE('',*,*,#4677,.F.);
#5986=ORIENTED_EDGE('',*,*,#4678,.T.);
#5987=ORIENTED_EDGE('',*,*,#4679,.F.);
#5988=ORIENTED_EDGE('',*,*,#4678,.F.);
#5989=ORIENTED_EDGE('',*,*,#4680,.F.);
#5990=ORIENTED_EDGE('',*,*,#4681,.T.);
#5991=ORIENTED_EDGE('',*,*,#4682,.F.);
#5992=ORIENTED_EDGE('',*,*,#4681,.F.);
#5993=ORIENTED_EDGE('',*,*,#4683,.F.);
#5994=ORIENTED_EDGE('',*,*,#4684,.T.);
#5995=ORIENTED_EDGE('',*,*,#4685,.F.);
#5996=ORIENTED_EDGE('',*,*,#4684,.F.);
#5997=ORIENTED_EDGE('',*,*,#4686,.F.);
#5998=ORIENTED_EDGE('',*,*,#4687,.T.);
#5999=ORIENTED_EDGE('',*,*,#4688,.F.);
#6000=ORIENTED_EDGE('',*,*,#4687,.F.);
#6001=ORIENTED_EDGE('',*,*,#4689,.F.);
#6002=ORIENTED_EDGE('',*,*,#4690,.T.);
#6003=ORIENTED_EDGE('',*,*,#4691,.F.);
#6004=ORIENTED_EDGE('',*,*,#4690,.F.);
#6005=ORIENTED_EDGE('',*,*,#4692,.F.);
#6006=ORIENTED_EDGE('',*,*,#4693,.T.);
#6007=ORIENTED_EDGE('',*,*,#4694,.F.);
#6008=ORIENTED_EDGE('',*,*,#4693,.F.);
#6009=ORIENTED_EDGE('',*,*,#4695,.F.);
#6010=ORIENTED_EDGE('',*,*,#4696,.T.);
#6011=ORIENTED_EDGE('',*,*,#4697,.F.);
#6012=ORIENTED_EDGE('',*,*,#4696,.F.);
#6013=ORIENTED_EDGE('',*,*,#4698,.F.);
#6014=ORIENTED_EDGE('',*,*,#4699,.F.);
#6015=ORIENTED_EDGE('',*,*,#4700,.T.);
#6016=ORIENTED_EDGE('',*,*,#4701,.F.);
#6017=ORIENTED_EDGE('',*,*,#4688,.T.);
#6018=ORIENTED_EDGE('',*,*,#4697,.T.);
#6019=ORIENTED_EDGE('',*,*,#4702,.F.);
#6020=ORIENTED_EDGE('',*,*,#4703,.F.);
#6021=ORIENTED_EDGE('',*,*,#4704,.F.);
#6022=ORIENTED_EDGE('',*,*,#4705,.F.);
#6023=ORIENTED_EDGE('',*,*,#4691,.T.);
#6024=ORIENTED_EDGE('',*,*,#4694,.T.);
#6025=ORIENTED_EDGE('',*,*,#4706,.F.);
#6026=ORIENTED_EDGE('',*,*,#4704,.T.);
#6027=ORIENTED_EDGE('',*,*,#4707,.F.);
#6028=ORIENTED_EDGE('',*,*,#4708,.F.);
#6029=ORIENTED_EDGE('',*,*,#4709,.F.);
#6030=ORIENTED_EDGE('',*,*,#4710,.T.);
#6031=ORIENTED_EDGE('',*,*,#4711,.F.);
#6032=ORIENTED_EDGE('',*,*,#4700,.F.);
#6033=ORIENTED_EDGE('',*,*,#4712,.T.);
#6034=ORIENTED_EDGE('',*,*,#4713,.F.);
#6035=ORIENTED_EDGE('',*,*,#4714,.F.);
#6036=ORIENTED_EDGE('',*,*,#4705,.T.);
#6037=ORIENTED_EDGE('',*,*,#4706,.T.);
#6038=ORIENTED_EDGE('',*,*,#4715,.T.);
#6039=ORIENTED_EDGE('',*,*,#4709,.T.);
#6040=ORIENTED_EDGE('',*,*,#4699,.T.);
#6041=ORIENTED_EDGE('',*,*,#4683,.T.);
#6042=ORIENTED_EDGE('',*,*,#4680,.T.);
#6043=ORIENTED_EDGE('',*,*,#4677,.T.);
#6044=ORIENTED_EDGE('',*,*,#4674,.T.);
#6045=ORIENTED_EDGE('',*,*,#4671,.T.);
#6046=ORIENTED_EDGE('',*,*,#4698,.T.);
#6047=ORIENTED_EDGE('',*,*,#4716,.T.);
#6048=ORIENTED_EDGE('',*,*,#4717,.F.);
#6049=ORIENTED_EDGE('',*,*,#4712,.F.);
#6050=ORIENTED_EDGE('',*,*,#4718,.T.);
#6051=ORIENTED_EDGE('',*,*,#4719,.F.);
#6052=ORIENTED_EDGE('',*,*,#4716,.F.);
#6053=ORIENTED_EDGE('',*,*,#4701,.T.);
#6054=ORIENTED_EDGE('',*,*,#4711,.T.);
#6055=ORIENTED_EDGE('',*,*,#4720,.T.);
#6056=ORIENTED_EDGE('',*,*,#4707,.T.);
#6057=ORIENTED_EDGE('',*,*,#4703,.T.);
#6058=ORIENTED_EDGE('',*,*,#4685,.T.);
#6059=ORIENTED_EDGE('',*,*,#4682,.T.);
#6060=ORIENTED_EDGE('',*,*,#4679,.T.);
#6061=ORIENTED_EDGE('',*,*,#4676,.T.);
#6062=ORIENTED_EDGE('',*,*,#4673,.T.);
#6063=ORIENTED_EDGE('',*,*,#4702,.T.);
#6064=ORIENTED_EDGE('',*,*,#4714,.T.);
#6065=ORIENTED_EDGE('',*,*,#4721,.F.);
#6066=ORIENTED_EDGE('',*,*,#4718,.F.);
#6067=ORIENTED_EDGE('',*,*,#4721,.T.);
#6068=ORIENTED_EDGE('',*,*,#4713,.T.);
#6069=ORIENTED_EDGE('',*,*,#4717,.T.);
#6070=ORIENTED_EDGE('',*,*,#4719,.T.);
#6071=ORIENTED_EDGE('',*,*,#4720,.F.);
#6072=ORIENTED_EDGE('',*,*,#4710,.F.);
#6073=ORIENTED_EDGE('',*,*,#4715,.F.);
#6074=ORIENTED_EDGE('',*,*,#4708,.T.);
#6075=ORIENTED_EDGE('',*,*,#4686,.T.);
#6076=ORIENTED_EDGE('',*,*,#4689,.T.);
#6077=ORIENTED_EDGE('',*,*,#4692,.T.);
#6078=ORIENTED_EDGE('',*,*,#4695,.T.);
#6079=ORIENTED_EDGE('',*,*,#4722,.F.);
#6080=ORIENTED_EDGE('',*,*,#4723,.T.);
#6081=ORIENTED_EDGE('',*,*,#4724,.T.);
#6082=ORIENTED_EDGE('',*,*,#4723,.F.);
#6083=ORIENTED_EDGE('',*,*,#4725,.F.);
#6084=ORIENTED_EDGE('',*,*,#4726,.T.);
#6085=ORIENTED_EDGE('',*,*,#4727,.T.);
#6086=ORIENTED_EDGE('',*,*,#4726,.F.);
#6087=ORIENTED_EDGE('',*,*,#4725,.T.);
#6088=ORIENTED_EDGE('',*,*,#4722,.T.);
#6089=ORIENTED_EDGE('',*,*,#4727,.F.);
#6090=ORIENTED_EDGE('',*,*,#4724,.F.);
#6091=ORIENTED_EDGE('',*,*,#4728,.F.);
#6092=ORIENTED_EDGE('',*,*,#4729,.F.);
#6093=ORIENTED_EDGE('',*,*,#4730,.F.);
#6094=ORIENTED_EDGE('',*,*,#4731,.F.);
#6095=ORIENTED_EDGE('',*,*,#4732,.F.);
#6096=ORIENTED_EDGE('',*,*,#4733,.F.);
#6097=ORIENTED_EDGE('',*,*,#4734,.F.);
#6098=ORIENTED_EDGE('',*,*,#4735,.F.);
#6099=ORIENTED_EDGE('',*,*,#4736,.F.);
#6100=ORIENTED_EDGE('',*,*,#4737,.F.);
#6101=ORIENTED_EDGE('',*,*,#4738,.F.);
#6102=ORIENTED_EDGE('',*,*,#4739,.F.);
#6103=ORIENTED_EDGE('',*,*,#4740,.F.);
#6104=ORIENTED_EDGE('',*,*,#4741,.F.);
#6105=ORIENTED_EDGE('',*,*,#4742,.F.);
#6106=ORIENTED_EDGE('',*,*,#4743,.F.);
#6107=ORIENTED_EDGE('',*,*,#4729,.T.);
#6108=ORIENTED_EDGE('',*,*,#4744,.F.);
#6109=ORIENTED_EDGE('',*,*,#4741,.T.);
#6110=ORIENTED_EDGE('',*,*,#4745,.F.);
#6111=ORIENTED_EDGE('',*,*,#4737,.T.);
#6112=ORIENTED_EDGE('',*,*,#4746,.F.);
#6113=ORIENTED_EDGE('',*,*,#4733,.T.);
#6114=ORIENTED_EDGE('',*,*,#4747,.F.);
#6115=ORIENTED_EDGE('',*,*,#4748,.F.);
#6116=ORIENTED_EDGE('',*,*,#4738,.T.);
#6117=ORIENTED_EDGE('',*,*,#4745,.T.);
#6118=ORIENTED_EDGE('',*,*,#4740,.T.);
#6119=ORIENTED_EDGE('',*,*,#4749,.F.);
#6120=ORIENTED_EDGE('',*,*,#4734,.T.);
#6121=ORIENTED_EDGE('',*,*,#4746,.T.);
#6122=ORIENTED_EDGE('',*,*,#4736,.T.);
#6123=ORIENTED_EDGE('',*,*,#4750,.F.);
#6124=ORIENTED_EDGE('',*,*,#4728,.T.);
#6125=ORIENTED_EDGE('',*,*,#4751,.F.);
#6126=ORIENTED_EDGE('',*,*,#4742,.T.);
#6127=ORIENTED_EDGE('',*,*,#4744,.T.);
#6128=ORIENTED_EDGE('',*,*,#4730,.T.);
#6129=ORIENTED_EDGE('',*,*,#4747,.T.);
#6130=ORIENTED_EDGE('',*,*,#4732,.T.);
#6131=ORIENTED_EDGE('',*,*,#4752,.F.);
#6132=ORIENTED_EDGE('',*,*,#4753,.F.);
#6133=ORIENTED_EDGE('',*,*,#4754,.T.);
#6134=ORIENTED_EDGE('',*,*,#4755,.F.);
#6135=ORIENTED_EDGE('',*,*,#4754,.F.);
#6136=ORIENTED_EDGE('',*,*,#4753,.T.);
#6137=ORIENTED_EDGE('',*,*,#4756,.T.);
#6138=ORIENTED_EDGE('',*,*,#4756,.F.);
#6139=ORIENTED_EDGE('',*,*,#4757,.T.);
#6140=ORIENTED_EDGE('',*,*,#4748,.T.);
#6141=ORIENTED_EDGE('',*,*,#4757,.F.);
#6142=ORIENTED_EDGE('',*,*,#4731,.T.);
#6143=ORIENTED_EDGE('',*,*,#4752,.T.);
#6144=ORIENTED_EDGE('',*,*,#4735,.T.);
#6145=ORIENTED_EDGE('',*,*,#4750,.T.);
#6146=ORIENTED_EDGE('',*,*,#4739,.T.);
#6147=ORIENTED_EDGE('',*,*,#4749,.T.);
#6148=ORIENTED_EDGE('',*,*,#4743,.T.);
#6149=ORIENTED_EDGE('',*,*,#4751,.T.);
#6150=ORIENTED_EDGE('',*,*,#4755,.T.);
#6151=ORIENTED_EDGE('',*,*,#4758,.F.);
#6152=ORIENTED_EDGE('',*,*,#4759,.F.);
#6153=ORIENTED_EDGE('',*,*,#4760,.F.);
#6154=ORIENTED_EDGE('',*,*,#4761,.F.);
#6155=ORIENTED_EDGE('',*,*,#4762,.F.);
#6156=ORIENTED_EDGE('',*,*,#4763,.F.);
#6157=ORIENTED_EDGE('',*,*,#4764,.F.);
#6158=ORIENTED_EDGE('',*,*,#4765,.F.);
#6159=ORIENTED_EDGE('',*,*,#4766,.F.);
#6160=ORIENTED_EDGE('',*,*,#4767,.F.);
#6161=ORIENTED_EDGE('',*,*,#4768,.F.);
#6162=ORIENTED_EDGE('',*,*,#4769,.F.);
#6163=ORIENTED_EDGE('',*,*,#4770,.F.);
#6164=ORIENTED_EDGE('',*,*,#4771,.F.);
#6165=ORIENTED_EDGE('',*,*,#4772,.F.);
#6166=ORIENTED_EDGE('',*,*,#4773,.F.);
#6167=ORIENTED_EDGE('',*,*,#4759,.T.);
#6168=ORIENTED_EDGE('',*,*,#4774,.F.);
#6169=ORIENTED_EDGE('',*,*,#4771,.T.);
#6170=ORIENTED_EDGE('',*,*,#4775,.F.);
#6171=ORIENTED_EDGE('',*,*,#4767,.T.);
#6172=ORIENTED_EDGE('',*,*,#4776,.F.);
#6173=ORIENTED_EDGE('',*,*,#4763,.T.);
#6174=ORIENTED_EDGE('',*,*,#4777,.F.);
#6175=ORIENTED_EDGE('',*,*,#4778,.T.);
#6176=ORIENTED_EDGE('',*,*,#4768,.T.);
#6177=ORIENTED_EDGE('',*,*,#4775,.T.);
#6178=ORIENTED_EDGE('',*,*,#4770,.T.);
#6179=ORIENTED_EDGE('',*,*,#4779,.F.);
#6180=ORIENTED_EDGE('',*,*,#4764,.T.);
#6181=ORIENTED_EDGE('',*,*,#4776,.T.);
#6182=ORIENTED_EDGE('',*,*,#4766,.T.);
#6183=ORIENTED_EDGE('',*,*,#4780,.F.);
#6184=ORIENTED_EDGE('',*,*,#4758,.T.);
#6185=ORIENTED_EDGE('',*,*,#4781,.F.);
#6186=ORIENTED_EDGE('',*,*,#4772,.T.);
#6187=ORIENTED_EDGE('',*,*,#4774,.T.);
#6188=ORIENTED_EDGE('',*,*,#4760,.T.);
#6189=ORIENTED_EDGE('',*,*,#4777,.T.);
#6190=ORIENTED_EDGE('',*,*,#4762,.T.);
#6191=ORIENTED_EDGE('',*,*,#4782,.F.);
#6192=ORIENTED_EDGE('',*,*,#4778,.F.);
#6193=ORIENTED_EDGE('',*,*,#4783,.T.);
#6194=ORIENTED_EDGE('',*,*,#4784,.T.);
#6195=ORIENTED_EDGE('',*,*,#4783,.F.);
#6196=ORIENTED_EDGE('',*,*,#4784,.F.);
#6197=ORIENTED_EDGE('',*,*,#4785,.F.);
#6198=ORIENTED_EDGE('',*,*,#4786,.F.);
#6199=ORIENTED_EDGE('',*,*,#4787,.T.);
#6200=ORIENTED_EDGE('',*,*,#4785,.T.);
#6201=ORIENTED_EDGE('',*,*,#4787,.F.);
#6202=ORIENTED_EDGE('',*,*,#4761,.T.);
#6203=ORIENTED_EDGE('',*,*,#4782,.T.);
#6204=ORIENTED_EDGE('',*,*,#4765,.T.);
#6205=ORIENTED_EDGE('',*,*,#4780,.T.);
#6206=ORIENTED_EDGE('',*,*,#4769,.T.);
#6207=ORIENTED_EDGE('',*,*,#4779,.T.);
#6208=ORIENTED_EDGE('',*,*,#4773,.T.);
#6209=ORIENTED_EDGE('',*,*,#4781,.T.);
#6210=ORIENTED_EDGE('',*,*,#4786,.T.);
#6211=ORIENTED_EDGE('',*,*,#4788,.F.);
#6212=ORIENTED_EDGE('',*,*,#4789,.T.);
#6213=ORIENTED_EDGE('',*,*,#4790,.F.);
#6214=ORIENTED_EDGE('',*,*,#4789,.F.);
#6215=ORIENTED_EDGE('',*,*,#4791,.F.);
#6216=ORIENTED_EDGE('',*,*,#4792,.T.);
#6217=ORIENTED_EDGE('',*,*,#4793,.F.);
#6218=ORIENTED_EDGE('',*,*,#4792,.F.);
#6219=ORIENTED_EDGE('',*,*,#4794,.F.);
#6220=ORIENTED_EDGE('',*,*,#4795,.T.);
#6221=ORIENTED_EDGE('',*,*,#4796,.F.);
#6222=ORIENTED_EDGE('',*,*,#4795,.F.);
#6223=ORIENTED_EDGE('',*,*,#4797,.F.);
#6224=ORIENTED_EDGE('',*,*,#4798,.T.);
#6225=ORIENTED_EDGE('',*,*,#4799,.F.);
#6226=ORIENTED_EDGE('',*,*,#4798,.F.);
#6227=ORIENTED_EDGE('',*,*,#4800,.F.);
#6228=ORIENTED_EDGE('',*,*,#4801,.T.);
#6229=ORIENTED_EDGE('',*,*,#4802,.F.);
#6230=ORIENTED_EDGE('',*,*,#4801,.F.);
#6231=ORIENTED_EDGE('',*,*,#4803,.F.);
#6232=ORIENTED_EDGE('',*,*,#4804,.T.);
#6233=ORIENTED_EDGE('',*,*,#4805,.F.);
#6234=ORIENTED_EDGE('',*,*,#4804,.F.);
#6235=ORIENTED_EDGE('',*,*,#4806,.F.);
#6236=ORIENTED_EDGE('',*,*,#4807,.T.);
#6237=ORIENTED_EDGE('',*,*,#4808,.F.);
#6238=ORIENTED_EDGE('',*,*,#4807,.F.);
#6239=ORIENTED_EDGE('',*,*,#4809,.F.);
#6240=ORIENTED_EDGE('',*,*,#4810,.T.);
#6241=ORIENTED_EDGE('',*,*,#4811,.F.);
#6242=ORIENTED_EDGE('',*,*,#4810,.F.);
#6243=ORIENTED_EDGE('',*,*,#4812,.F.);
#6244=ORIENTED_EDGE('',*,*,#4813,.T.);
#6245=ORIENTED_EDGE('',*,*,#4814,.F.);
#6246=ORIENTED_EDGE('',*,*,#4813,.F.);
#6247=ORIENTED_EDGE('',*,*,#4815,.F.);
#6248=ORIENTED_EDGE('',*,*,#4816,.F.);
#6249=ORIENTED_EDGE('',*,*,#4817,.T.);
#6250=ORIENTED_EDGE('',*,*,#4818,.F.);
#6251=ORIENTED_EDGE('',*,*,#4805,.T.);
#6252=ORIENTED_EDGE('',*,*,#4814,.T.);
#6253=ORIENTED_EDGE('',*,*,#4819,.F.);
#6254=ORIENTED_EDGE('',*,*,#4820,.F.);
#6255=ORIENTED_EDGE('',*,*,#4821,.F.);
#6256=ORIENTED_EDGE('',*,*,#4822,.F.);
#6257=ORIENTED_EDGE('',*,*,#4808,.T.);
#6258=ORIENTED_EDGE('',*,*,#4811,.T.);
#6259=ORIENTED_EDGE('',*,*,#4823,.F.);
#6260=ORIENTED_EDGE('',*,*,#4821,.T.);
#6261=ORIENTED_EDGE('',*,*,#4824,.F.);
#6262=ORIENTED_EDGE('',*,*,#4825,.F.);
#6263=ORIENTED_EDGE('',*,*,#4826,.F.);
#6264=ORIENTED_EDGE('',*,*,#4827,.T.);
#6265=ORIENTED_EDGE('',*,*,#4828,.F.);
#6266=ORIENTED_EDGE('',*,*,#4817,.F.);
#6267=ORIENTED_EDGE('',*,*,#4829,.T.);
#6268=ORIENTED_EDGE('',*,*,#4830,.F.);
#6269=ORIENTED_EDGE('',*,*,#4831,.F.);
#6270=ORIENTED_EDGE('',*,*,#4822,.T.);
#6271=ORIENTED_EDGE('',*,*,#4823,.T.);
#6272=ORIENTED_EDGE('',*,*,#4832,.T.);
#6273=ORIENTED_EDGE('',*,*,#4826,.T.);
#6274=ORIENTED_EDGE('',*,*,#4816,.T.);
#6275=ORIENTED_EDGE('',*,*,#4800,.T.);
#6276=ORIENTED_EDGE('',*,*,#4797,.T.);
#6277=ORIENTED_EDGE('',*,*,#4794,.T.);
#6278=ORIENTED_EDGE('',*,*,#4791,.T.);
#6279=ORIENTED_EDGE('',*,*,#4788,.T.);
#6280=ORIENTED_EDGE('',*,*,#4815,.T.);
#6281=ORIENTED_EDGE('',*,*,#4833,.T.);
#6282=ORIENTED_EDGE('',*,*,#4834,.F.);
#6283=ORIENTED_EDGE('',*,*,#4829,.F.);
#6284=ORIENTED_EDGE('',*,*,#4835,.T.);
#6285=ORIENTED_EDGE('',*,*,#4836,.F.);
#6286=ORIENTED_EDGE('',*,*,#4833,.F.);
#6287=ORIENTED_EDGE('',*,*,#4818,.T.);
#6288=ORIENTED_EDGE('',*,*,#4828,.T.);
#6289=ORIENTED_EDGE('',*,*,#4837,.T.);
#6290=ORIENTED_EDGE('',*,*,#4824,.T.);
#6291=ORIENTED_EDGE('',*,*,#4820,.T.);
#6292=ORIENTED_EDGE('',*,*,#4802,.T.);
#6293=ORIENTED_EDGE('',*,*,#4799,.T.);
#6294=ORIENTED_EDGE('',*,*,#4796,.T.);
#6295=ORIENTED_EDGE('',*,*,#4793,.T.);
#6296=ORIENTED_EDGE('',*,*,#4790,.T.);
#6297=ORIENTED_EDGE('',*,*,#4819,.T.);
#6298=ORIENTED_EDGE('',*,*,#4831,.T.);
#6299=ORIENTED_EDGE('',*,*,#4838,.F.);
#6300=ORIENTED_EDGE('',*,*,#4835,.F.);
#6301=ORIENTED_EDGE('',*,*,#4838,.T.);
#6302=ORIENTED_EDGE('',*,*,#4830,.T.);
#6303=ORIENTED_EDGE('',*,*,#4834,.T.);
#6304=ORIENTED_EDGE('',*,*,#4836,.T.);
#6305=ORIENTED_EDGE('',*,*,#4837,.F.);
#6306=ORIENTED_EDGE('',*,*,#4827,.F.);
#6307=ORIENTED_EDGE('',*,*,#4832,.F.);
#6308=ORIENTED_EDGE('',*,*,#4825,.T.);
#6309=ORIENTED_EDGE('',*,*,#4803,.T.);
#6310=ORIENTED_EDGE('',*,*,#4806,.T.);
#6311=ORIENTED_EDGE('',*,*,#4809,.T.);
#6312=ORIENTED_EDGE('',*,*,#4812,.T.);
#6313=ORIENTED_EDGE('',*,*,#4839,.F.);
#6314=ORIENTED_EDGE('',*,*,#4840,.T.);
#6315=ORIENTED_EDGE('',*,*,#4841,.T.);
#6316=ORIENTED_EDGE('',*,*,#4840,.F.);
#6317=ORIENTED_EDGE('',*,*,#4842,.F.);
#6318=ORIENTED_EDGE('',*,*,#4843,.T.);
#6319=ORIENTED_EDGE('',*,*,#4844,.T.);
#6320=ORIENTED_EDGE('',*,*,#4843,.F.);
#6321=ORIENTED_EDGE('',*,*,#4842,.T.);
#6322=ORIENTED_EDGE('',*,*,#4839,.T.);
#6323=ORIENTED_EDGE('',*,*,#4844,.F.);
#6324=ORIENTED_EDGE('',*,*,#4841,.F.);
#6325=ORIENTED_EDGE('',*,*,#4845,.F.);
#6326=ORIENTED_EDGE('',*,*,#4846,.T.);
#6327=ORIENTED_EDGE('',*,*,#4847,.T.);
#6328=ORIENTED_EDGE('',*,*,#4846,.F.);
#6329=ORIENTED_EDGE('',*,*,#4848,.F.);
#6330=ORIENTED_EDGE('',*,*,#4849,.T.);
#6331=ORIENTED_EDGE('',*,*,#4850,.T.);
#6332=ORIENTED_EDGE('',*,*,#4849,.F.);
#6333=ORIENTED_EDGE('',*,*,#4848,.T.);
#6334=ORIENTED_EDGE('',*,*,#4845,.T.);
#6335=ORIENTED_EDGE('',*,*,#4850,.F.);
#6336=ORIENTED_EDGE('',*,*,#4847,.F.);
#6337=ORIENTED_EDGE('',*,*,#4851,.F.);
#6338=ORIENTED_EDGE('',*,*,#4852,.T.);
#6339=ORIENTED_EDGE('',*,*,#4853,.T.);
#6340=ORIENTED_EDGE('',*,*,#4852,.F.);
#6341=ORIENTED_EDGE('',*,*,#4854,.F.);
#6342=ORIENTED_EDGE('',*,*,#4855,.T.);
#6343=ORIENTED_EDGE('',*,*,#4856,.T.);
#6344=ORIENTED_EDGE('',*,*,#4855,.F.);
#6345=ORIENTED_EDGE('',*,*,#4854,.T.);
#6346=ORIENTED_EDGE('',*,*,#4851,.T.);
#6347=ORIENTED_EDGE('',*,*,#4856,.F.);
#6348=ORIENTED_EDGE('',*,*,#4853,.F.);
#6349=ORIENTED_EDGE('',*,*,#4857,.F.);
#6350=ORIENTED_EDGE('',*,*,#4858,.T.);
#6351=ORIENTED_EDGE('',*,*,#4859,.T.);
#6352=ORIENTED_EDGE('',*,*,#4858,.F.);
#6353=ORIENTED_EDGE('',*,*,#4860,.F.);
#6354=ORIENTED_EDGE('',*,*,#4861,.T.);
#6355=ORIENTED_EDGE('',*,*,#4862,.T.);
#6356=ORIENTED_EDGE('',*,*,#4861,.F.);
#6357=ORIENTED_EDGE('',*,*,#4860,.T.);
#6358=ORIENTED_EDGE('',*,*,#4857,.T.);
#6359=ORIENTED_EDGE('',*,*,#4862,.F.);
#6360=ORIENTED_EDGE('',*,*,#4859,.F.);
#6361=ORIENTED_EDGE('',*,*,#4863,.F.);
#6362=ORIENTED_EDGE('',*,*,#4864,.T.);
#6363=ORIENTED_EDGE('',*,*,#4865,.T.);
#6364=ORIENTED_EDGE('',*,*,#4864,.F.);
#6365=ORIENTED_EDGE('',*,*,#4866,.F.);
#6366=ORIENTED_EDGE('',*,*,#4867,.T.);
#6367=ORIENTED_EDGE('',*,*,#4868,.T.);
#6368=ORIENTED_EDGE('',*,*,#4867,.F.);
#6369=ORIENTED_EDGE('',*,*,#4866,.T.);
#6370=ORIENTED_EDGE('',*,*,#4863,.T.);
#6371=ORIENTED_EDGE('',*,*,#4868,.F.);
#6372=ORIENTED_EDGE('',*,*,#4865,.F.);
#6373=ORIENTED_EDGE('',*,*,#4869,.F.);
#6374=ORIENTED_EDGE('',*,*,#4870,.F.);
#6375=ORIENTED_EDGE('',*,*,#4871,.F.);
#6376=ORIENTED_EDGE('',*,*,#4872,.F.);
#6377=ORIENTED_EDGE('',*,*,#4873,.F.);
#6378=ORIENTED_EDGE('',*,*,#4874,.F.);
#6379=ORIENTED_EDGE('',*,*,#4875,.F.);
#6380=ORIENTED_EDGE('',*,*,#4876,.F.);
#6381=ORIENTED_EDGE('',*,*,#4877,.F.);
#6382=ORIENTED_EDGE('',*,*,#4878,.F.);
#6383=ORIENTED_EDGE('',*,*,#4879,.F.);
#6384=ORIENTED_EDGE('',*,*,#4880,.F.);
#6385=ORIENTED_EDGE('',*,*,#4881,.F.);
#6386=ORIENTED_EDGE('',*,*,#4882,.F.);
#6387=ORIENTED_EDGE('',*,*,#4883,.F.);
#6388=ORIENTED_EDGE('',*,*,#4884,.F.);
#6389=ORIENTED_EDGE('',*,*,#4870,.T.);
#6390=ORIENTED_EDGE('',*,*,#4885,.F.);
#6391=ORIENTED_EDGE('',*,*,#4882,.T.);
#6392=ORIENTED_EDGE('',*,*,#4886,.F.);
#6393=ORIENTED_EDGE('',*,*,#4878,.T.);
#6394=ORIENTED_EDGE('',*,*,#4887,.F.);
#6395=ORIENTED_EDGE('',*,*,#4874,.T.);
#6396=ORIENTED_EDGE('',*,*,#4888,.F.);
#6397=ORIENTED_EDGE('',*,*,#4889,.F.);
#6398=ORIENTED_EDGE('',*,*,#4879,.T.);
#6399=ORIENTED_EDGE('',*,*,#4886,.T.);
#6400=ORIENTED_EDGE('',*,*,#4881,.T.);
#6401=ORIENTED_EDGE('',*,*,#4890,.F.);
#6402=ORIENTED_EDGE('',*,*,#4875,.T.);
#6403=ORIENTED_EDGE('',*,*,#4887,.T.);
#6404=ORIENTED_EDGE('',*,*,#4877,.T.);
#6405=ORIENTED_EDGE('',*,*,#4891,.F.);
#6406=ORIENTED_EDGE('',*,*,#4869,.T.);
#6407=ORIENTED_EDGE('',*,*,#4892,.F.);
#6408=ORIENTED_EDGE('',*,*,#4883,.T.);
#6409=ORIENTED_EDGE('',*,*,#4885,.T.);
#6410=ORIENTED_EDGE('',*,*,#4871,.T.);
#6411=ORIENTED_EDGE('',*,*,#4888,.T.);
#6412=ORIENTED_EDGE('',*,*,#4873,.T.);
#6413=ORIENTED_EDGE('',*,*,#4893,.F.);
#6414=ORIENTED_EDGE('',*,*,#4894,.F.);
#6415=ORIENTED_EDGE('',*,*,#4895,.T.);
#6416=ORIENTED_EDGE('',*,*,#4896,.F.);
#6417=ORIENTED_EDGE('',*,*,#4895,.F.);
#6418=ORIENTED_EDGE('',*,*,#4894,.T.);
#6419=ORIENTED_EDGE('',*,*,#4897,.T.);
#6420=ORIENTED_EDGE('',*,*,#4897,.F.);
#6421=ORIENTED_EDGE('',*,*,#4898,.T.);
#6422=ORIENTED_EDGE('',*,*,#4889,.T.);
#6423=ORIENTED_EDGE('',*,*,#4898,.F.);
#6424=ORIENTED_EDGE('',*,*,#4872,.T.);
#6425=ORIENTED_EDGE('',*,*,#4893,.T.);
#6426=ORIENTED_EDGE('',*,*,#4876,.T.);
#6427=ORIENTED_EDGE('',*,*,#4891,.T.);
#6428=ORIENTED_EDGE('',*,*,#4880,.T.);
#6429=ORIENTED_EDGE('',*,*,#4890,.T.);
#6430=ORIENTED_EDGE('',*,*,#4884,.T.);
#6431=ORIENTED_EDGE('',*,*,#4892,.T.);
#6432=ORIENTED_EDGE('',*,*,#4896,.T.);
#6433=ORIENTED_EDGE('',*,*,#4899,.F.);
#6434=ORIENTED_EDGE('',*,*,#4900,.F.);
#6435=ORIENTED_EDGE('',*,*,#4901,.F.);
#6436=ORIENTED_EDGE('',*,*,#4902,.F.);
#6437=ORIENTED_EDGE('',*,*,#4903,.F.);
#6438=ORIENTED_EDGE('',*,*,#4904,.F.);
#6439=ORIENTED_EDGE('',*,*,#4905,.F.);
#6440=ORIENTED_EDGE('',*,*,#4906,.F.);
#6441=ORIENTED_EDGE('',*,*,#4907,.F.);
#6442=ORIENTED_EDGE('',*,*,#4908,.F.);
#6443=ORIENTED_EDGE('',*,*,#4909,.F.);
#6444=ORIENTED_EDGE('',*,*,#4910,.F.);
#6445=ORIENTED_EDGE('',*,*,#4911,.F.);
#6446=ORIENTED_EDGE('',*,*,#4912,.F.);
#6447=ORIENTED_EDGE('',*,*,#4913,.F.);
#6448=ORIENTED_EDGE('',*,*,#4914,.F.);
#6449=ORIENTED_EDGE('',*,*,#4900,.T.);
#6450=ORIENTED_EDGE('',*,*,#4915,.F.);
#6451=ORIENTED_EDGE('',*,*,#4912,.T.);
#6452=ORIENTED_EDGE('',*,*,#4916,.F.);
#6453=ORIENTED_EDGE('',*,*,#4908,.T.);
#6454=ORIENTED_EDGE('',*,*,#4917,.F.);
#6455=ORIENTED_EDGE('',*,*,#4904,.T.);
#6456=ORIENTED_EDGE('',*,*,#4918,.F.);
#6457=ORIENTED_EDGE('',*,*,#4919,.T.);
#6458=ORIENTED_EDGE('',*,*,#4909,.T.);
#6459=ORIENTED_EDGE('',*,*,#4916,.T.);
#6460=ORIENTED_EDGE('',*,*,#4911,.T.);
#6461=ORIENTED_EDGE('',*,*,#4920,.F.);
#6462=ORIENTED_EDGE('',*,*,#4905,.T.);
#6463=ORIENTED_EDGE('',*,*,#4917,.T.);
#6464=ORIENTED_EDGE('',*,*,#4907,.T.);
#6465=ORIENTED_EDGE('',*,*,#4921,.F.);
#6466=ORIENTED_EDGE('',*,*,#4899,.T.);
#6467=ORIENTED_EDGE('',*,*,#4922,.F.);
#6468=ORIENTED_EDGE('',*,*,#4913,.T.);
#6469=ORIENTED_EDGE('',*,*,#4915,.T.);
#6470=ORIENTED_EDGE('',*,*,#4901,.T.);
#6471=ORIENTED_EDGE('',*,*,#4918,.T.);
#6472=ORIENTED_EDGE('',*,*,#4903,.T.);
#6473=ORIENTED_EDGE('',*,*,#4923,.F.);
#6474=ORIENTED_EDGE('',*,*,#4919,.F.);
#6475=ORIENTED_EDGE('',*,*,#4924,.T.);
#6476=ORIENTED_EDGE('',*,*,#4925,.T.);
#6477=ORIENTED_EDGE('',*,*,#4924,.F.);
#6478=ORIENTED_EDGE('',*,*,#4925,.F.);
#6479=ORIENTED_EDGE('',*,*,#4926,.F.);
#6480=ORIENTED_EDGE('',*,*,#4927,.F.);
#6481=ORIENTED_EDGE('',*,*,#4928,.T.);
#6482=ORIENTED_EDGE('',*,*,#4926,.T.);
#6483=ORIENTED_EDGE('',*,*,#4928,.F.);
#6484=ORIENTED_EDGE('',*,*,#4902,.T.);
#6485=ORIENTED_EDGE('',*,*,#4923,.T.);
#6486=ORIENTED_EDGE('',*,*,#4906,.T.);
#6487=ORIENTED_EDGE('',*,*,#4921,.T.);
#6488=ORIENTED_EDGE('',*,*,#4910,.T.);
#6489=ORIENTED_EDGE('',*,*,#4920,.T.);
#6490=ORIENTED_EDGE('',*,*,#4914,.T.);
#6491=ORIENTED_EDGE('',*,*,#4922,.T.);
#6492=ORIENTED_EDGE('',*,*,#4927,.T.);
#6493=ORIENTED_EDGE('',*,*,#4929,.F.);
#6494=ORIENTED_EDGE('',*,*,#4930,.F.);
#6495=ORIENTED_EDGE('',*,*,#4931,.F.);
#6496=ORIENTED_EDGE('',*,*,#4932,.T.);
#6497=ORIENTED_EDGE('',*,*,#4933,.F.);
#6498=ORIENTED_EDGE('',*,*,#4934,.F.);
#6499=ORIENTED_EDGE('',*,*,#4935,.F.);
#6500=ORIENTED_EDGE('',*,*,#4936,.F.);
#6501=ORIENTED_EDGE('',*,*,#4937,.F.);
#6502=ORIENTED_EDGE('',*,*,#4938,.F.);
#6503=ORIENTED_EDGE('',*,*,#4939,.F.);
#6504=ORIENTED_EDGE('',*,*,#4940,.F.);
#6505=ORIENTED_EDGE('',*,*,#4929,.T.);
#6506=ORIENTED_EDGE('',*,*,#4941,.T.);
#6507=ORIENTED_EDGE('',*,*,#4933,.T.);
#6508=ORIENTED_EDGE('',*,*,#4942,.T.);
#6509=ORIENTED_EDGE('',*,*,#4932,.F.);
#6510=ORIENTED_EDGE('',*,*,#4943,.F.);
#6511=ORIENTED_EDGE('',*,*,#4934,.T.);
#6512=ORIENTED_EDGE('',*,*,#4941,.F.);
#6513=ORIENTED_EDGE('',*,*,#4930,.T.);
#6514=ORIENTED_EDGE('',*,*,#4942,.F.);
#6515=ORIENTED_EDGE('',*,*,#4936,.T.);
#6516=ORIENTED_EDGE('',*,*,#4944,.F.);
#6517=ORIENTED_EDGE('',*,*,#4945,.T.);
#6518=ORIENTED_EDGE('',*,*,#4946,.F.);
#6519=ORIENTED_EDGE('',*,*,#4947,.F.);
#6520=ORIENTED_EDGE('',*,*,#4940,.T.);
#6521=ORIENTED_EDGE('',*,*,#4939,.T.);
#6522=ORIENTED_EDGE('',*,*,#4948,.T.);
#6523=ORIENTED_EDGE('',*,*,#4949,.F.);
#6524=ORIENTED_EDGE('',*,*,#4945,.F.);
#6525=ORIENTED_EDGE('',*,*,#4937,.T.);
#6526=ORIENTED_EDGE('',*,*,#4947,.T.);
#6527=ORIENTED_EDGE('',*,*,#4950,.F.);
#6528=ORIENTED_EDGE('',*,*,#4951,.F.);
#6529=ORIENTED_EDGE('',*,*,#4948,.F.);
#6530=ORIENTED_EDGE('',*,*,#4938,.T.);
#6531=ORIENTED_EDGE('',*,*,#4951,.T.);
#6532=ORIENTED_EDGE('',*,*,#4952,.F.);
#6533=ORIENTED_EDGE('',*,*,#4949,.T.);
#6534=ORIENTED_EDGE('',*,*,#4952,.T.);
#6535=ORIENTED_EDGE('',*,*,#4950,.T.);
#6536=ORIENTED_EDGE('',*,*,#4946,.T.);
#6537=ORIENTED_EDGE('',*,*,#4931,.T.);
#6538=ORIENTED_EDGE('',*,*,#4944,.T.);
#6539=ORIENTED_EDGE('',*,*,#4935,.T.);
#6540=ORIENTED_EDGE('',*,*,#4943,.T.);
#6541=ORIENTED_EDGE('',*,*,#4953,.F.);
#6542=ORIENTED_EDGE('',*,*,#4954,.F.);
#6543=ORIENTED_EDGE('',*,*,#4955,.T.);
#6544=ORIENTED_EDGE('',*,*,#4956,.F.);
#6545=ORIENTED_EDGE('',*,*,#4957,.F.);
#6546=ORIENTED_EDGE('',*,*,#4955,.F.);
#6547=ORIENTED_EDGE('',*,*,#4956,.T.);
#6548=ORIENTED_EDGE('',*,*,#4957,.T.);
#6549=ORIENTED_EDGE('',*,*,#4958,.T.);
#6550=ORIENTED_EDGE('',*,*,#4959,.T.);
#6551=ORIENTED_EDGE('',*,*,#4958,.F.);
#6552=ORIENTED_EDGE('',*,*,#4960,.T.);
#6553=ORIENTED_EDGE('',*,*,#4961,.T.);
#6554=ORIENTED_EDGE('',*,*,#4962,.F.);
#6555=ORIENTED_EDGE('',*,*,#4961,.F.);
#6556=ORIENTED_EDGE('',*,*,#4962,.T.);
#6557=ORIENTED_EDGE('',*,*,#4963,.T.);
#6558=ORIENTED_EDGE('',*,*,#4964,.F.);
#6559=ORIENTED_EDGE('',*,*,#4963,.F.);
#6560=ORIENTED_EDGE('',*,*,#4959,.F.);
#6561=ORIENTED_EDGE('',*,*,#4964,.T.);
#6562=ORIENTED_EDGE('',*,*,#4965,.F.);
#6563=ORIENTED_EDGE('',*,*,#4966,.T.);
#6564=ORIENTED_EDGE('',*,*,#4953,.T.);
#6565=ORIENTED_EDGE('',*,*,#4954,.T.);
#6566=ORIENTED_EDGE('',*,*,#4966,.F.);
#6567=ORIENTED_EDGE('',*,*,#4965,.T.);
#6568=ORIENTED_EDGE('',*,*,#4967,.F.);
#6569=ORIENTED_EDGE('',*,*,#4967,.T.);
#6570=ORIENTED_EDGE('',*,*,#4968,.T.);
#6571=ORIENTED_EDGE('',*,*,#4960,.F.);
#6572=ORIENTED_EDGE('',*,*,#4968,.F.);
#6573=ORIENTED_EDGE('',*,*,#4969,.F.);
#6574=ORIENTED_EDGE('',*,*,#4970,.F.);
#6575=ORIENTED_EDGE('',*,*,#4971,.T.);
#6576=ORIENTED_EDGE('',*,*,#4972,.F.);
#6577=ORIENTED_EDGE('',*,*,#4973,.F.);
#6578=ORIENTED_EDGE('',*,*,#4971,.F.);
#6579=ORIENTED_EDGE('',*,*,#4974,.T.);
#6580=ORIENTED_EDGE('',*,*,#4975,.T.);
#6581=ORIENTED_EDGE('',*,*,#4972,.T.);
#6582=ORIENTED_EDGE('',*,*,#4973,.T.);
#6583=ORIENTED_EDGE('',*,*,#4975,.F.);
#6584=ORIENTED_EDGE('',*,*,#4976,.F.);
#6585=ORIENTED_EDGE('',*,*,#4977,.T.);
#6586=ORIENTED_EDGE('',*,*,#4978,.F.);
#6587=ORIENTED_EDGE('',*,*,#4979,.T.);
#6588=ORIENTED_EDGE('',*,*,#4976,.T.);
#6589=ORIENTED_EDGE('',*,*,#4979,.F.);
#6590=ORIENTED_EDGE('',*,*,#4980,.F.);
#6591=ORIENTED_EDGE('',*,*,#4981,.T.);
#6592=ORIENTED_EDGE('',*,*,#4978,.T.);
#6593=ORIENTED_EDGE('',*,*,#4981,.F.);
#6594=ORIENTED_EDGE('',*,*,#4982,.F.);
#6595=ORIENTED_EDGE('',*,*,#4983,.T.);
#6596=ORIENTED_EDGE('',*,*,#4980,.T.);
#6597=ORIENTED_EDGE('',*,*,#4983,.F.);
#6598=ORIENTED_EDGE('',*,*,#4982,.T.);
#6599=ORIENTED_EDGE('',*,*,#4974,.F.);
#6600=ORIENTED_EDGE('',*,*,#4969,.T.);
#6601=ORIENTED_EDGE('',*,*,#4970,.T.);
#6602=ORIENTED_EDGE('',*,*,#4984,.T.);
#6603=ORIENTED_EDGE('',*,*,#4977,.F.);
#6604=ORIENTED_EDGE('',*,*,#4984,.F.);
#6605=ORIENTED_EDGE('',*,*,#4985,.T.);
#6606=ORIENTED_EDGE('',*,*,#4985,.F.);
#6607=ORIENTED_EDGE('',*,*,#4986,.T.);
#6608=ORIENTED_EDGE('',*,*,#4986,.F.);
#6609=ORIENTED_EDGE('',*,*,#4987,.T.);
#6610=ORIENTED_EDGE('',*,*,#4987,.F.);
#6611=ORIENTED_EDGE('',*,*,#4988,.T.);
#6612=ORIENTED_EDGE('',*,*,#4988,.F.);
#6613=ORIENTED_EDGE('',*,*,#4989,.T.);
#6614=ORIENTED_EDGE('',*,*,#4989,.F.);
#6615=ORIENTED_EDGE('',*,*,#4990,.T.);
#6616=ORIENTED_EDGE('',*,*,#4990,.F.);
#6617=ORIENTED_EDGE('',*,*,#4991,.T.);
#6618=ORIENTED_EDGE('',*,*,#4991,.F.);
#6619=ORIENTED_EDGE('',*,*,#4992,.T.);
#6620=ORIENTED_EDGE('',*,*,#4992,.F.);
#6621=ORIENTED_EDGE('',*,*,#4993,.F.);
#6622=ORIENTED_EDGE('',*,*,#4994,.F.);
#6623=ORIENTED_EDGE('',*,*,#4995,.F.);
#6624=ORIENTED_EDGE('',*,*,#4996,.F.);
#6625=ORIENTED_EDGE('',*,*,#4995,.T.);
#6626=ORIENTED_EDGE('',*,*,#4997,.F.);
#6627=ORIENTED_EDGE('',*,*,#4998,.T.);
#6628=ORIENTED_EDGE('',*,*,#4999,.F.);
#6629=ORIENTED_EDGE('',*,*,#5000,.T.);
#6630=ORIENTED_EDGE('',*,*,#5001,.F.);
#6631=ORIENTED_EDGE('',*,*,#5002,.T.);
#6632=ORIENTED_EDGE('',*,*,#5003,.T.);
#6633=ORIENTED_EDGE('',*,*,#5004,.F.);
#6634=ORIENTED_EDGE('',*,*,#5003,.F.);
#6635=ORIENTED_EDGE('',*,*,#5005,.T.);
#6636=ORIENTED_EDGE('',*,*,#5006,.F.);
#6637=ORIENTED_EDGE('',*,*,#5007,.T.);
#6638=ORIENTED_EDGE('',*,*,#5008,.F.);
#6639=ORIENTED_EDGE('',*,*,#5009,.T.);
#6640=ORIENTED_EDGE('',*,*,#5010,.F.);
#6641=ORIENTED_EDGE('',*,*,#5011,.T.);
#6642=ORIENTED_EDGE('',*,*,#5012,.F.);
#6643=ORIENTED_EDGE('',*,*,#5013,.T.);
#6644=ORIENTED_EDGE('',*,*,#5014,.F.);
#6645=ORIENTED_EDGE('',*,*,#4994,.T.);
#6646=ORIENTED_EDGE('',*,*,#5015,.T.);
#6647=ORIENTED_EDGE('',*,*,#5016,.T.);
#6648=ORIENTED_EDGE('',*,*,#4997,.T.);
#6649=ORIENTED_EDGE('',*,*,#5017,.F.);
#6650=ORIENTED_EDGE('',*,*,#5018,.F.);
#6651=ORIENTED_EDGE('',*,*,#4998,.F.);
#6652=ORIENTED_EDGE('',*,*,#5016,.F.);
#6653=ORIENTED_EDGE('',*,*,#5018,.T.);
#6654=ORIENTED_EDGE('',*,*,#5019,.T.);
#6655=ORIENTED_EDGE('',*,*,#5020,.T.);
#6656=ORIENTED_EDGE('',*,*,#4999,.T.);
#6657=ORIENTED_EDGE('',*,*,#5021,.F.);
#6658=ORIENTED_EDGE('',*,*,#5022,.F.);
#6659=ORIENTED_EDGE('',*,*,#5000,.F.);
#6660=ORIENTED_EDGE('',*,*,#5020,.F.);
#6661=ORIENTED_EDGE('',*,*,#5022,.T.);
#6662=ORIENTED_EDGE('',*,*,#5023,.T.);
#6663=ORIENTED_EDGE('',*,*,#5024,.T.);
#6664=ORIENTED_EDGE('',*,*,#5001,.T.);
#6665=ORIENTED_EDGE('',*,*,#5025,.F.);
#6666=ORIENTED_EDGE('',*,*,#5026,.F.);
#6667=ORIENTED_EDGE('',*,*,#5005,.F.);
#6668=ORIENTED_EDGE('',*,*,#5002,.F.);
#6669=ORIENTED_EDGE('',*,*,#5024,.F.);
#6670=ORIENTED_EDGE('',*,*,#5027,.F.);
#6671=ORIENTED_EDGE('',*,*,#5026,.T.);
#6672=ORIENTED_EDGE('',*,*,#5028,.T.);
#6673=ORIENTED_EDGE('',*,*,#5029,.T.);
#6674=ORIENTED_EDGE('',*,*,#5006,.T.);
#6675=ORIENTED_EDGE('',*,*,#5030,.F.);
#6676=ORIENTED_EDGE('',*,*,#5031,.F.);
#6677=ORIENTED_EDGE('',*,*,#5007,.F.);
#6678=ORIENTED_EDGE('',*,*,#5029,.F.);
#6679=ORIENTED_EDGE('',*,*,#5031,.T.);
#6680=ORIENTED_EDGE('',*,*,#5032,.T.);
#6681=ORIENTED_EDGE('',*,*,#5033,.T.);
#6682=ORIENTED_EDGE('',*,*,#5008,.T.);
#6683=ORIENTED_EDGE('',*,*,#5034,.F.);
#6684=ORIENTED_EDGE('',*,*,#5035,.F.);
#6685=ORIENTED_EDGE('',*,*,#5009,.F.);
#6686=ORIENTED_EDGE('',*,*,#5033,.F.);
#6687=ORIENTED_EDGE('',*,*,#5035,.T.);
#6688=ORIENTED_EDGE('',*,*,#5036,.T.);
#6689=ORIENTED_EDGE('',*,*,#5037,.T.);
#6690=ORIENTED_EDGE('',*,*,#5010,.T.);
#6691=ORIENTED_EDGE('',*,*,#5011,.F.);
#6692=ORIENTED_EDGE('',*,*,#5037,.F.);
#6693=ORIENTED_EDGE('',*,*,#5038,.F.);
#6694=ORIENTED_EDGE('',*,*,#5039,.F.);
#6695=ORIENTED_EDGE('',*,*,#5040,.F.);
#6696=ORIENTED_EDGE('',*,*,#5041,.T.);
#6697=ORIENTED_EDGE('',*,*,#5027,.T.);
#6698=ORIENTED_EDGE('',*,*,#5023,.F.);
#6699=ORIENTED_EDGE('',*,*,#5021,.T.);
#6700=ORIENTED_EDGE('',*,*,#5019,.F.);
#6701=ORIENTED_EDGE('',*,*,#5017,.T.);
#6702=ORIENTED_EDGE('',*,*,#5015,.F.);
#6703=ORIENTED_EDGE('',*,*,#4993,.T.);
#6704=ORIENTED_EDGE('',*,*,#5042,.F.);
#6705=ORIENTED_EDGE('',*,*,#5043,.T.);
#6706=ORIENTED_EDGE('',*,*,#5044,.F.);
#6707=ORIENTED_EDGE('',*,*,#5038,.T.);
#6708=ORIENTED_EDGE('',*,*,#5036,.F.);
#6709=ORIENTED_EDGE('',*,*,#5034,.T.);
#6710=ORIENTED_EDGE('',*,*,#5032,.F.);
#6711=ORIENTED_EDGE('',*,*,#5030,.T.);
#6712=ORIENTED_EDGE('',*,*,#5028,.F.);
#6713=ORIENTED_EDGE('',*,*,#5025,.T.);
#6714=ORIENTED_EDGE('',*,*,#5041,.F.);
#6715=ORIENTED_EDGE('',*,*,#4996,.T.);
#6716=ORIENTED_EDGE('',*,*,#5014,.T.);
#6717=ORIENTED_EDGE('',*,*,#5045,.T.);
#6718=ORIENTED_EDGE('',*,*,#5042,.T.);
#6719=ORIENTED_EDGE('',*,*,#5013,.F.);
#6720=ORIENTED_EDGE('',*,*,#5046,.F.);
#6721=ORIENTED_EDGE('',*,*,#5043,.F.);
#6722=ORIENTED_EDGE('',*,*,#5045,.F.);
#6723=ORIENTED_EDGE('',*,*,#5004,.T.);
#6724=ORIENTED_EDGE('',*,*,#5040,.T.);
#6725=ORIENTED_EDGE('',*,*,#5039,.T.);
#6726=ORIENTED_EDGE('',*,*,#5044,.T.);
#6727=ORIENTED_EDGE('',*,*,#5046,.T.);
#6728=ORIENTED_EDGE('',*,*,#5012,.T.);
#6729=ORIENTED_EDGE('',*,*,#5047,.F.);
#6730=ORIENTED_EDGE('',*,*,#5048,.T.);
#6731=ORIENTED_EDGE('',*,*,#5049,.F.);
#6732=ORIENTED_EDGE('',*,*,#5050,.T.);
#6733=ORIENTED_EDGE('',*,*,#5047,.T.);
#6734=ORIENTED_EDGE('',*,*,#5050,.F.);
#6735=ORIENTED_EDGE('',*,*,#5049,.T.);
#6736=ORIENTED_EDGE('',*,*,#5051,.F.);
#6737=ORIENTED_EDGE('',*,*,#5051,.T.);
#6738=ORIENTED_EDGE('',*,*,#5052,.T.);
#6739=ORIENTED_EDGE('',*,*,#5048,.F.);
#6740=ORIENTED_EDGE('',*,*,#5052,.F.);
#6741=ORIENTED_EDGE('',*,*,#5053,.F.);
#6742=ORIENTED_EDGE('',*,*,#5054,.T.);
#6743=ORIENTED_EDGE('',*,*,#5055,.F.);
#6744=ORIENTED_EDGE('',*,*,#5056,.T.);
#6745=ORIENTED_EDGE('',*,*,#5053,.T.);
#6746=ORIENTED_EDGE('',*,*,#5056,.F.);
#6747=ORIENTED_EDGE('',*,*,#5055,.T.);
#6748=ORIENTED_EDGE('',*,*,#5057,.F.);
#6749=ORIENTED_EDGE('',*,*,#5057,.T.);
#6750=ORIENTED_EDGE('',*,*,#5058,.T.);
#6751=ORIENTED_EDGE('',*,*,#5054,.F.);
#6752=ORIENTED_EDGE('',*,*,#5058,.F.);
#6753=ORIENTED_EDGE('',*,*,#5059,.T.);
#6754=ORIENTED_EDGE('',*,*,#5060,.T.);
#6755=ORIENTED_EDGE('',*,*,#5061,.T.);
#6756=ORIENTED_EDGE('',*,*,#5062,.F.);
#6757=ORIENTED_EDGE('',*,*,#5063,.T.);
#6758=ORIENTED_EDGE('',*,*,#5064,.T.);
#6759=ORIENTED_EDGE('',*,*,#5065,.T.);
#6760=ORIENTED_EDGE('',*,*,#5060,.F.);
#6761=ORIENTED_EDGE('',*,*,#5066,.T.);
#6762=ORIENTED_EDGE('',*,*,#5067,.T.);
#6763=ORIENTED_EDGE('',*,*,#5068,.T.);
#6764=ORIENTED_EDGE('',*,*,#5064,.F.);
#6765=ORIENTED_EDGE('',*,*,#5069,.T.);
#6766=ORIENTED_EDGE('',*,*,#5070,.T.);
#6767=ORIENTED_EDGE('',*,*,#5071,.T.);
#6768=ORIENTED_EDGE('',*,*,#5067,.F.);
#6769=ORIENTED_EDGE('',*,*,#5072,.T.);
#6770=ORIENTED_EDGE('',*,*,#5073,.T.);
#6771=ORIENTED_EDGE('',*,*,#5074,.T.);
#6772=ORIENTED_EDGE('',*,*,#5070,.F.);
#6773=ORIENTED_EDGE('',*,*,#5075,.T.);
#6774=ORIENTED_EDGE('',*,*,#5062,.T.);
#6775=ORIENTED_EDGE('',*,*,#5076,.T.);
#6776=ORIENTED_EDGE('',*,*,#5073,.F.);
#6777=ORIENTED_EDGE('',*,*,#5075,.F.);
#6778=ORIENTED_EDGE('',*,*,#5072,.F.);
#6779=ORIENTED_EDGE('',*,*,#5069,.F.);
#6780=ORIENTED_EDGE('',*,*,#5066,.F.);
#6781=ORIENTED_EDGE('',*,*,#5063,.F.);
#6782=ORIENTED_EDGE('',*,*,#5059,.F.);
#6783=ORIENTED_EDGE('',*,*,#5076,.F.);
#6784=ORIENTED_EDGE('',*,*,#5061,.F.);
#6785=ORIENTED_EDGE('',*,*,#5065,.F.);
#6786=ORIENTED_EDGE('',*,*,#5068,.F.);
#6787=ORIENTED_EDGE('',*,*,#5071,.F.);
#6788=ORIENTED_EDGE('',*,*,#5074,.F.);
#6789=ORIENTED_EDGE('',*,*,#5077,.T.);
#6790=ORIENTED_EDGE('',*,*,#5078,.T.);
#6791=ORIENTED_EDGE('',*,*,#5077,.F.);
#6792=ORIENTED_EDGE('',*,*,#5079,.T.);
#6793=ORIENTED_EDGE('',*,*,#5080,.T.);
#6794=ORIENTED_EDGE('',*,*,#5079,.F.);
#6795=ORIENTED_EDGE('',*,*,#5080,.F.);
#6796=ORIENTED_EDGE('',*,*,#5081,.F.);
#6797=ORIENTED_EDGE('',*,*,#5082,.F.);
#6798=ORIENTED_EDGE('',*,*,#5083,.T.);
#6799=ORIENTED_EDGE('',*,*,#5081,.T.);
#6800=ORIENTED_EDGE('',*,*,#5083,.F.);
#6801=ORIENTED_EDGE('',*,*,#5084,.F.);
#6802=ORIENTED_EDGE('',*,*,#5085,.T.);
#6803=ORIENTED_EDGE('',*,*,#5082,.T.);
#6804=ORIENTED_EDGE('',*,*,#5085,.F.);
#6805=ORIENTED_EDGE('',*,*,#5086,.F.);
#6806=ORIENTED_EDGE('',*,*,#5087,.T.);
#6807=ORIENTED_EDGE('',*,*,#5084,.T.);
#6808=ORIENTED_EDGE('',*,*,#5087,.F.);
#6809=ORIENTED_EDGE('',*,*,#5086,.T.);
#6810=ORIENTED_EDGE('',*,*,#5088,.F.);
#6811=ORIENTED_EDGE('',*,*,#5089,.F.);
#6812=ORIENTED_EDGE('',*,*,#5090,.T.);
#6813=ORIENTED_EDGE('',*,*,#5088,.T.);
#6814=ORIENTED_EDGE('',*,*,#5090,.F.);
#6815=ORIENTED_EDGE('',*,*,#5091,.F.);
#6816=ORIENTED_EDGE('',*,*,#5092,.T.);
#6817=ORIENTED_EDGE('',*,*,#5089,.T.);
#6818=ORIENTED_EDGE('',*,*,#5092,.F.);
#6819=ORIENTED_EDGE('',*,*,#5078,.F.);
#6820=ORIENTED_EDGE('',*,*,#5093,.T.);
#6821=ORIENTED_EDGE('',*,*,#5091,.T.);
#6822=ORIENTED_EDGE('',*,*,#5093,.F.);
#6823=ORIENTED_EDGE('',*,*,#5094,.F.);
#6824=ORIENTED_EDGE('',*,*,#5095,.F.);
#6825=ORIENTED_EDGE('',*,*,#5096,.T.);
#6826=ORIENTED_EDGE('',*,*,#5097,.F.);
#6827=ORIENTED_EDGE('',*,*,#5098,.F.);
#6828=ORIENTED_EDGE('',*,*,#5096,.F.);
#6829=ORIENTED_EDGE('',*,*,#5097,.T.);
#6830=ORIENTED_EDGE('',*,*,#5098,.T.);
#6831=ORIENTED_EDGE('',*,*,#5099,.T.);
#6832=ORIENTED_EDGE('',*,*,#5100,.T.);
#6833=ORIENTED_EDGE('',*,*,#5099,.F.);
#6834=ORIENTED_EDGE('',*,*,#5101,.T.);
#6835=ORIENTED_EDGE('',*,*,#5102,.T.);
#6836=ORIENTED_EDGE('',*,*,#5103,.F.);
#6837=ORIENTED_EDGE('',*,*,#5102,.F.);
#6838=ORIENTED_EDGE('',*,*,#5103,.T.);
#6839=ORIENTED_EDGE('',*,*,#5104,.T.);
#6840=ORIENTED_EDGE('',*,*,#5105,.F.);
#6841=ORIENTED_EDGE('',*,*,#5104,.F.);
#6842=ORIENTED_EDGE('',*,*,#5100,.F.);
#6843=ORIENTED_EDGE('',*,*,#5105,.T.);
#6844=ORIENTED_EDGE('',*,*,#5106,.F.);
#6845=ORIENTED_EDGE('',*,*,#5107,.T.);
#6846=ORIENTED_EDGE('',*,*,#5094,.T.);
#6847=ORIENTED_EDGE('',*,*,#5095,.T.);
#6848=ORIENTED_EDGE('',*,*,#5107,.F.);
#6849=ORIENTED_EDGE('',*,*,#5106,.T.);
#6850=ORIENTED_EDGE('',*,*,#5108,.F.);
#6851=ORIENTED_EDGE('',*,*,#5108,.T.);
#6852=ORIENTED_EDGE('',*,*,#5109,.T.);
#6853=ORIENTED_EDGE('',*,*,#5101,.F.);
#6854=ORIENTED_EDGE('',*,*,#5109,.F.);
#6855=ORIENTED_EDGE('',*,*,#5110,.F.);
#6856=ORIENTED_EDGE('',*,*,#5111,.F.);
#6857=ORIENTED_EDGE('',*,*,#5112,.T.);
#6858=ORIENTED_EDGE('',*,*,#5113,.F.);
#6859=ORIENTED_EDGE('',*,*,#5114,.F.);
#6860=ORIENTED_EDGE('',*,*,#5112,.F.);
#6861=ORIENTED_EDGE('',*,*,#5115,.T.);
#6862=ORIENTED_EDGE('',*,*,#5116,.T.);
#6863=ORIENTED_EDGE('',*,*,#5113,.T.);
#6864=ORIENTED_EDGE('',*,*,#5114,.T.);
#6865=ORIENTED_EDGE('',*,*,#5116,.F.);
#6866=ORIENTED_EDGE('',*,*,#5117,.F.);
#6867=ORIENTED_EDGE('',*,*,#5118,.T.);
#6868=ORIENTED_EDGE('',*,*,#5119,.F.);
#6869=ORIENTED_EDGE('',*,*,#5120,.T.);
#6870=ORIENTED_EDGE('',*,*,#5117,.T.);
#6871=ORIENTED_EDGE('',*,*,#5120,.F.);
#6872=ORIENTED_EDGE('',*,*,#5121,.F.);
#6873=ORIENTED_EDGE('',*,*,#5122,.T.);
#6874=ORIENTED_EDGE('',*,*,#5119,.T.);
#6875=ORIENTED_EDGE('',*,*,#5122,.F.);
#6876=ORIENTED_EDGE('',*,*,#5123,.F.);
#6877=ORIENTED_EDGE('',*,*,#5124,.T.);
#6878=ORIENTED_EDGE('',*,*,#5121,.T.);
#6879=ORIENTED_EDGE('',*,*,#5124,.F.);
#6880=ORIENTED_EDGE('',*,*,#5123,.T.);
#6881=ORIENTED_EDGE('',*,*,#5115,.F.);
#6882=ORIENTED_EDGE('',*,*,#5110,.T.);
#6883=ORIENTED_EDGE('',*,*,#5111,.T.);
#6884=ORIENTED_EDGE('',*,*,#5125,.T.);
#6885=ORIENTED_EDGE('',*,*,#5118,.F.);
#6886=ORIENTED_EDGE('',*,*,#5125,.F.);
#6887=ORIENTED_EDGE('',*,*,#5126,.T.);
#6888=ORIENTED_EDGE('',*,*,#5126,.F.);
#6889=ORIENTED_EDGE('',*,*,#5127,.T.);
#6890=ORIENTED_EDGE('',*,*,#5127,.F.);
#6891=ORIENTED_EDGE('',*,*,#5128,.T.);
#6892=ORIENTED_EDGE('',*,*,#5128,.F.);
#6893=ORIENTED_EDGE('',*,*,#5129,.T.);
#6894=ORIENTED_EDGE('',*,*,#5129,.F.);
#6895=ORIENTED_EDGE('',*,*,#5130,.T.);
#6896=ORIENTED_EDGE('',*,*,#5130,.F.);
#6897=ORIENTED_EDGE('',*,*,#5131,.T.);
#6898=ORIENTED_EDGE('',*,*,#5131,.F.);
#6899=ORIENTED_EDGE('',*,*,#5132,.T.);
#6900=ORIENTED_EDGE('',*,*,#5132,.F.);
#6901=ORIENTED_EDGE('',*,*,#5133,.F.);
#6902=ORIENTED_EDGE('',*,*,#5134,.F.);
#6903=ORIENTED_EDGE('',*,*,#5135,.F.);
#6904=ORIENTED_EDGE('',*,*,#5136,.F.);
#6905=ORIENTED_EDGE('',*,*,#5135,.T.);
#6906=ORIENTED_EDGE('',*,*,#5137,.F.);
#6907=ORIENTED_EDGE('',*,*,#5138,.T.);
#6908=ORIENTED_EDGE('',*,*,#5139,.F.);
#6909=ORIENTED_EDGE('',*,*,#5140,.T.);
#6910=ORIENTED_EDGE('',*,*,#5141,.F.);
#6911=ORIENTED_EDGE('',*,*,#5142,.T.);
#6912=ORIENTED_EDGE('',*,*,#5143,.F.);
#6913=ORIENTED_EDGE('',*,*,#5142,.F.);
#6914=ORIENTED_EDGE('',*,*,#5144,.F.);
#6915=ORIENTED_EDGE('',*,*,#5145,.T.);
#6916=ORIENTED_EDGE('',*,*,#5146,.F.);
#6917=ORIENTED_EDGE('',*,*,#5147,.T.);
#6918=ORIENTED_EDGE('',*,*,#5148,.F.);
#6919=ORIENTED_EDGE('',*,*,#5149,.T.);
#6920=ORIENTED_EDGE('',*,*,#5150,.F.);
#6921=ORIENTED_EDGE('',*,*,#5151,.T.);
#6922=ORIENTED_EDGE('',*,*,#5152,.F.);
#6923=ORIENTED_EDGE('',*,*,#5134,.T.);
#6924=ORIENTED_EDGE('',*,*,#5153,.T.);
#6925=ORIENTED_EDGE('',*,*,#5154,.T.);
#6926=ORIENTED_EDGE('',*,*,#5137,.T.);
#6927=ORIENTED_EDGE('',*,*,#5155,.F.);
#6928=ORIENTED_EDGE('',*,*,#5156,.F.);
#6929=ORIENTED_EDGE('',*,*,#5138,.F.);
#6930=ORIENTED_EDGE('',*,*,#5154,.F.);
#6931=ORIENTED_EDGE('',*,*,#5156,.T.);
#6932=ORIENTED_EDGE('',*,*,#5157,.T.);
#6933=ORIENTED_EDGE('',*,*,#5158,.T.);
#6934=ORIENTED_EDGE('',*,*,#5139,.T.);
#6935=ORIENTED_EDGE('',*,*,#5159,.F.);
#6936=ORIENTED_EDGE('',*,*,#5160,.F.);
#6937=ORIENTED_EDGE('',*,*,#5140,.F.);
#6938=ORIENTED_EDGE('',*,*,#5158,.F.);
#6939=ORIENTED_EDGE('',*,*,#5160,.T.);
#6940=ORIENTED_EDGE('',*,*,#5161,.T.);
#6941=ORIENTED_EDGE('',*,*,#5162,.T.);
#6942=ORIENTED_EDGE('',*,*,#5163,.T.);
#6943=ORIENTED_EDGE('',*,*,#5144,.T.);
#6944=ORIENTED_EDGE('',*,*,#5141,.T.);
#6945=ORIENTED_EDGE('',*,*,#5164,.F.);
#6946=ORIENTED_EDGE('',*,*,#5165,.F.);
#6947=ORIENTED_EDGE('',*,*,#5145,.F.);
#6948=ORIENTED_EDGE('',*,*,#5163,.F.);
#6949=ORIENTED_EDGE('',*,*,#5165,.T.);
#6950=ORIENTED_EDGE('',*,*,#5166,.T.);
#6951=ORIENTED_EDGE('',*,*,#5167,.T.);
#6952=ORIENTED_EDGE('',*,*,#5146,.T.);
#6953=ORIENTED_EDGE('',*,*,#5168,.F.);
#6954=ORIENTED_EDGE('',*,*,#5169,.F.);
#6955=ORIENTED_EDGE('',*,*,#5147,.F.);
#6956=ORIENTED_EDGE('',*,*,#5167,.F.);
#6957=ORIENTED_EDGE('',*,*,#5169,.T.);
#6958=ORIENTED_EDGE('',*,*,#5170,.T.);
#6959=ORIENTED_EDGE('',*,*,#5171,.T.);
#6960=ORIENTED_EDGE('',*,*,#5148,.T.);
#6961=ORIENTED_EDGE('',*,*,#5149,.F.);
#6962=ORIENTED_EDGE('',*,*,#5171,.F.);
#6963=ORIENTED_EDGE('',*,*,#5172,.F.);
#6964=ORIENTED_EDGE('',*,*,#5173,.F.);
#6965=ORIENTED_EDGE('',*,*,#5174,.F.);
#6966=ORIENTED_EDGE('',*,*,#5175,.T.);
#6967=ORIENTED_EDGE('',*,*,#5161,.F.);
#6968=ORIENTED_EDGE('',*,*,#5159,.T.);
#6969=ORIENTED_EDGE('',*,*,#5157,.F.);
#6970=ORIENTED_EDGE('',*,*,#5155,.T.);
#6971=ORIENTED_EDGE('',*,*,#5153,.F.);
#6972=ORIENTED_EDGE('',*,*,#5133,.T.);
#6973=ORIENTED_EDGE('',*,*,#5176,.F.);
#6974=ORIENTED_EDGE('',*,*,#5177,.T.);
#6975=ORIENTED_EDGE('',*,*,#5178,.F.);
#6976=ORIENTED_EDGE('',*,*,#5172,.T.);
#6977=ORIENTED_EDGE('',*,*,#5170,.F.);
#6978=ORIENTED_EDGE('',*,*,#5168,.T.);
#6979=ORIENTED_EDGE('',*,*,#5166,.F.);
#6980=ORIENTED_EDGE('',*,*,#5164,.T.);
#6981=ORIENTED_EDGE('',*,*,#5162,.F.);
#6982=ORIENTED_EDGE('',*,*,#5175,.F.);
#6983=ORIENTED_EDGE('',*,*,#5136,.T.);
#6984=ORIENTED_EDGE('',*,*,#5152,.T.);
#6985=ORIENTED_EDGE('',*,*,#5179,.T.);
#6986=ORIENTED_EDGE('',*,*,#5176,.T.);
#6987=ORIENTED_EDGE('',*,*,#5151,.F.);
#6988=ORIENTED_EDGE('',*,*,#5180,.F.);
#6989=ORIENTED_EDGE('',*,*,#5177,.F.);
#6990=ORIENTED_EDGE('',*,*,#5179,.F.);
#6991=ORIENTED_EDGE('',*,*,#5143,.T.);
#6992=ORIENTED_EDGE('',*,*,#5174,.T.);
#6993=ORIENTED_EDGE('',*,*,#5173,.T.);
#6994=ORIENTED_EDGE('',*,*,#5178,.T.);
#6995=ORIENTED_EDGE('',*,*,#5180,.T.);
#6996=ORIENTED_EDGE('',*,*,#5150,.T.);
#6997=ORIENTED_EDGE('',*,*,#5181,.F.);
#6998=ORIENTED_EDGE('',*,*,#5182,.T.);
#6999=ORIENTED_EDGE('',*,*,#5183,.F.);
#7000=ORIENTED_EDGE('',*,*,#5184,.T.);
#7001=ORIENTED_EDGE('',*,*,#5181,.T.);
#7002=ORIENTED_EDGE('',*,*,#5184,.F.);
#7003=ORIENTED_EDGE('',*,*,#5183,.T.);
#7004=ORIENTED_EDGE('',*,*,#5185,.F.);
#7005=ORIENTED_EDGE('',*,*,#5185,.T.);
#7006=ORIENTED_EDGE('',*,*,#5186,.T.);
#7007=ORIENTED_EDGE('',*,*,#5182,.F.);
#7008=ORIENTED_EDGE('',*,*,#5186,.F.);
#7009=ORIENTED_EDGE('',*,*,#5187,.F.);
#7010=ORIENTED_EDGE('',*,*,#5188,.T.);
#7011=ORIENTED_EDGE('',*,*,#5189,.F.);
#7012=ORIENTED_EDGE('',*,*,#5190,.T.);
#7013=ORIENTED_EDGE('',*,*,#5187,.T.);
#7014=ORIENTED_EDGE('',*,*,#5190,.F.);
#7015=ORIENTED_EDGE('',*,*,#5189,.T.);
#7016=ORIENTED_EDGE('',*,*,#5191,.F.);
#7017=ORIENTED_EDGE('',*,*,#5191,.T.);
#7018=ORIENTED_EDGE('',*,*,#5192,.T.);
#7019=ORIENTED_EDGE('',*,*,#5188,.F.);
#7020=ORIENTED_EDGE('',*,*,#5192,.F.);
#7021=ORIENTED_EDGE('',*,*,#5193,.T.);
#7022=ORIENTED_EDGE('',*,*,#5194,.T.);
#7023=ORIENTED_EDGE('',*,*,#5195,.T.);
#7024=ORIENTED_EDGE('',*,*,#5196,.F.);
#7025=ORIENTED_EDGE('',*,*,#5197,.T.);
#7026=ORIENTED_EDGE('',*,*,#5198,.T.);
#7027=ORIENTED_EDGE('',*,*,#5199,.T.);
#7028=ORIENTED_EDGE('',*,*,#5194,.F.);
#7029=ORIENTED_EDGE('',*,*,#5200,.T.);
#7030=ORIENTED_EDGE('',*,*,#5201,.T.);
#7031=ORIENTED_EDGE('',*,*,#5202,.T.);
#7032=ORIENTED_EDGE('',*,*,#5198,.F.);
#7033=ORIENTED_EDGE('',*,*,#5203,.T.);
#7034=ORIENTED_EDGE('',*,*,#5204,.T.);
#7035=ORIENTED_EDGE('',*,*,#5205,.T.);
#7036=ORIENTED_EDGE('',*,*,#5201,.F.);
#7037=ORIENTED_EDGE('',*,*,#5206,.T.);
#7038=ORIENTED_EDGE('',*,*,#5207,.T.);
#7039=ORIENTED_EDGE('',*,*,#5208,.T.);
#7040=ORIENTED_EDGE('',*,*,#5204,.F.);
#7041=ORIENTED_EDGE('',*,*,#5209,.T.);
#7042=ORIENTED_EDGE('',*,*,#5196,.T.);
#7043=ORIENTED_EDGE('',*,*,#5210,.T.);
#7044=ORIENTED_EDGE('',*,*,#5207,.F.);
#7045=ORIENTED_EDGE('',*,*,#5209,.F.);
#7046=ORIENTED_EDGE('',*,*,#5206,.F.);
#7047=ORIENTED_EDGE('',*,*,#5203,.F.);
#7048=ORIENTED_EDGE('',*,*,#5200,.F.);
#7049=ORIENTED_EDGE('',*,*,#5197,.F.);
#7050=ORIENTED_EDGE('',*,*,#5193,.F.);
#7051=ORIENTED_EDGE('',*,*,#5210,.F.);
#7052=ORIENTED_EDGE('',*,*,#5195,.F.);
#7053=ORIENTED_EDGE('',*,*,#5199,.F.);
#7054=ORIENTED_EDGE('',*,*,#5202,.F.);
#7055=ORIENTED_EDGE('',*,*,#5205,.F.);
#7056=ORIENTED_EDGE('',*,*,#5208,.F.);
#7057=ORIENTED_EDGE('',*,*,#5211,.F.);
#7058=ORIENTED_EDGE('',*,*,#5212,.F.);
#7059=ORIENTED_EDGE('',*,*,#5213,.F.);
#7060=ORIENTED_EDGE('',*,*,#5214,.T.);
#7061=ORIENTED_EDGE('',*,*,#5212,.T.);
#7062=ORIENTED_EDGE('',*,*,#5214,.F.);
#7063=ORIENTED_EDGE('',*,*,#5215,.F.);
#7064=ORIENTED_EDGE('',*,*,#5216,.T.);
#7065=ORIENTED_EDGE('',*,*,#5213,.T.);
#7066=ORIENTED_EDGE('',*,*,#5216,.F.);
#7067=ORIENTED_EDGE('',*,*,#5217,.F.);
#7068=ORIENTED_EDGE('',*,*,#5218,.T.);
#7069=ORIENTED_EDGE('',*,*,#5215,.T.);
#7070=ORIENTED_EDGE('',*,*,#5218,.F.);
#7071=ORIENTED_EDGE('',*,*,#5217,.T.);
#7072=ORIENTED_EDGE('',*,*,#5219,.F.);
#7073=ORIENTED_EDGE('',*,*,#5220,.F.);
#7074=ORIENTED_EDGE('',*,*,#5221,.T.);
#7075=ORIENTED_EDGE('',*,*,#5219,.T.);
#7076=ORIENTED_EDGE('',*,*,#5221,.F.);
#7077=ORIENTED_EDGE('',*,*,#5211,.T.);
#7078=ORIENTED_EDGE('',*,*,#5222,.T.);
#7079=ORIENTED_EDGE('',*,*,#5220,.T.);
#7080=ORIENTED_EDGE('',*,*,#5222,.F.);
#7081=ORIENTED_EDGE('',*,*,#5223,.F.);
#7082=ORIENTED_EDGE('',*,*,#5224,.T.);
#7083=ORIENTED_EDGE('',*,*,#5225,.T.);
#7084=ORIENTED_EDGE('',*,*,#5224,.F.);
#7085=ORIENTED_EDGE('',*,*,#5225,.F.);
#7086=ORIENTED_EDGE('',*,*,#5226,.T.);
#7087=ORIENTED_EDGE('',*,*,#5227,.F.);
#7088=ORIENTED_EDGE('',*,*,#5228,.F.);
#7089=ORIENTED_EDGE('',*,*,#5229,.F.);
#7090=ORIENTED_EDGE('',*,*,#5226,.F.);
#7091=ORIENTED_EDGE('',*,*,#5230,.T.);
#7092=ORIENTED_EDGE('',*,*,#5228,.T.);
#7093=ORIENTED_EDGE('',*,*,#5230,.F.);
#7094=ORIENTED_EDGE('',*,*,#5229,.T.);
#7095=ORIENTED_EDGE('',*,*,#5231,.T.);
#7096=ORIENTED_EDGE('',*,*,#5232,.T.);
#7097=ORIENTED_EDGE('',*,*,#5231,.F.);
#7098=ORIENTED_EDGE('',*,*,#5233,.F.);
#7099=ORIENTED_EDGE('',*,*,#5234,.T.);
#7100=ORIENTED_EDGE('',*,*,#5235,.T.);
#7101=ORIENTED_EDGE('',*,*,#5234,.F.);
#7102=ORIENTED_EDGE('',*,*,#5235,.F.);
#7103=ORIENTED_EDGE('',*,*,#5223,.T.);
#7104=ORIENTED_EDGE('',*,*,#5236,.F.);
#7105=ORIENTED_EDGE('',*,*,#5237,.T.);
#7106=ORIENTED_EDGE('',*,*,#5227,.T.);
#7107=ORIENTED_EDGE('',*,*,#5237,.F.);
#7108=ORIENTED_EDGE('',*,*,#5236,.T.);
#7109=ORIENTED_EDGE('',*,*,#5232,.F.);
#7110=ORIENTED_EDGE('',*,*,#5233,.T.);
#7111=ORIENTED_EDGE('',*,*,#5238,.F.);
#7112=ORIENTED_EDGE('',*,*,#5239,.T.);
#7113=ORIENTED_EDGE('',*,*,#5240,.F.);
#7114=ORIENTED_EDGE('',*,*,#5239,.F.);
#7115=ORIENTED_EDGE('',*,*,#5238,.T.);
#7116=ORIENTED_EDGE('',*,*,#5241,.F.);
#7117=ORIENTED_EDGE('',*,*,#5241,.T.);
#7118=ORIENTED_EDGE('',*,*,#5242,.T.);
#7119=ORIENTED_EDGE('',*,*,#5243,.T.);
#7120=ORIENTED_EDGE('',*,*,#5242,.F.);
#7121=ORIENTED_EDGE('',*,*,#5244,.F.);
#7122=ORIENTED_EDGE('',*,*,#5245,.T.);
#7123=ORIENTED_EDGE('',*,*,#5246,.T.);
#7124=ORIENTED_EDGE('',*,*,#5245,.F.);
#7125=ORIENTED_EDGE('',*,*,#5244,.T.);
#7126=ORIENTED_EDGE('',*,*,#5240,.T.);
#7127=ORIENTED_EDGE('',*,*,#5246,.F.);
#7128=ORIENTED_EDGE('',*,*,#5243,.F.);
#7129=ORIENTED_EDGE('',*,*,#5247,.F.);
#7130=ORIENTED_EDGE('',*,*,#5248,.T.);
#7131=ORIENTED_EDGE('',*,*,#5249,.T.);
#7132=ORIENTED_EDGE('',*,*,#5248,.F.);
#7133=ORIENTED_EDGE('',*,*,#5250,.F.);
#7134=ORIENTED_EDGE('',*,*,#5251,.T.);
#7135=ORIENTED_EDGE('',*,*,#5252,.T.);
#7136=ORIENTED_EDGE('',*,*,#5251,.F.);
#7137=ORIENTED_EDGE('',*,*,#5250,.T.);
#7138=ORIENTED_EDGE('',*,*,#5247,.T.);
#7139=ORIENTED_EDGE('',*,*,#5252,.F.);
#7140=ORIENTED_EDGE('',*,*,#5249,.F.);
#7141=ORIENTED_EDGE('',*,*,#5253,.F.);
#7142=ORIENTED_EDGE('',*,*,#5254,.T.);
#7143=ORIENTED_EDGE('',*,*,#5255,.T.);
#7144=ORIENTED_EDGE('',*,*,#5254,.F.);
#7145=ORIENTED_EDGE('',*,*,#5253,.T.);
#7146=ORIENTED_EDGE('',*,*,#5255,.F.);
#7147=ORIENTED_EDGE('',*,*,#5256,.F.);
#7148=ORIENTED_EDGE('',*,*,#5257,.T.);
#7149=ORIENTED_EDGE('',*,*,#5258,.T.);
#7150=ORIENTED_EDGE('',*,*,#5257,.F.);
#7151=ORIENTED_EDGE('',*,*,#5256,.T.);
#7152=ORIENTED_EDGE('',*,*,#5258,.F.);
#7153=ORIENTED_EDGE('',*,*,#5259,.F.);
#7154=ORIENTED_EDGE('',*,*,#5260,.T.);
#7155=ORIENTED_EDGE('',*,*,#5261,.T.);
#7156=ORIENTED_EDGE('',*,*,#5260,.F.);
#7157=ORIENTED_EDGE('',*,*,#5262,.F.);
#7158=ORIENTED_EDGE('',*,*,#5263,.T.);
#7159=ORIENTED_EDGE('',*,*,#5264,.T.);
#7160=ORIENTED_EDGE('',*,*,#5263,.F.);
#7161=ORIENTED_EDGE('',*,*,#5262,.T.);
#7162=ORIENTED_EDGE('',*,*,#5259,.T.);
#7163=ORIENTED_EDGE('',*,*,#5264,.F.);
#7164=ORIENTED_EDGE('',*,*,#5261,.F.);
#7165=ORIENTED_EDGE('',*,*,#5265,.F.);
#7166=ORIENTED_EDGE('',*,*,#5266,.F.);
#7167=ORIENTED_EDGE('',*,*,#5267,.F.);
#7168=ORIENTED_EDGE('',*,*,#5268,.T.);
#7169=ORIENTED_EDGE('',*,*,#5269,.F.);
#7170=ORIENTED_EDGE('',*,*,#5270,.F.);
#7171=ORIENTED_EDGE('',*,*,#5271,.F.);
#7172=ORIENTED_EDGE('',*,*,#5272,.F.);
#7173=ORIENTED_EDGE('',*,*,#5268,.F.);
#7174=ORIENTED_EDGE('',*,*,#5273,.F.);
#7175=ORIENTED_EDGE('',*,*,#5274,.F.);
#7176=ORIENTED_EDGE('',*,*,#5275,.T.);
#7177=ORIENTED_EDGE('',*,*,#5276,.F.);
#7178=ORIENTED_EDGE('',*,*,#5277,.F.);
#7179=ORIENTED_EDGE('',*,*,#5278,.F.);
#7180=ORIENTED_EDGE('',*,*,#5275,.F.);
#7181=ORIENTED_EDGE('',*,*,#5279,.F.);
#7182=ORIENTED_EDGE('',*,*,#5280,.T.);
#7183=ORIENTED_EDGE('',*,*,#5266,.T.);
#7184=ORIENTED_EDGE('',*,*,#5281,.T.);
#7185=ORIENTED_EDGE('',*,*,#5282,.F.);
#7186=ORIENTED_EDGE('',*,*,#5281,.F.);
#7187=ORIENTED_EDGE('',*,*,#5265,.T.);
#7188=ORIENTED_EDGE('',*,*,#5267,.T.);
#7189=ORIENTED_EDGE('',*,*,#5280,.F.);
#7190=ORIENTED_EDGE('',*,*,#5277,.T.);
#7191=ORIENTED_EDGE('',*,*,#5276,.T.);
#7192=ORIENTED_EDGE('',*,*,#5278,.T.);
#7193=ORIENTED_EDGE('',*,*,#5283,.T.);
#7194=ORIENTED_EDGE('',*,*,#5284,.T.);
#7195=ORIENTED_EDGE('',*,*,#5285,.T.);
#7196=ORIENTED_EDGE('',*,*,#5286,.T.);
#7197=ORIENTED_EDGE('',*,*,#5287,.T.);
#7198=ORIENTED_EDGE('',*,*,#5288,.T.);
#7199=ORIENTED_EDGE('',*,*,#5284,.F.);
#7200=ORIENTED_EDGE('',*,*,#5283,.F.);
#7201=ORIENTED_EDGE('',*,*,#5285,.F.);
#7202=ORIENTED_EDGE('',*,*,#5289,.T.);
#7203=ORIENTED_EDGE('',*,*,#5290,.F.);
#7204=ORIENTED_EDGE('',*,*,#5291,.F.);
#7205=ORIENTED_EDGE('',*,*,#5289,.F.);
#7206=ORIENTED_EDGE('',*,*,#5292,.F.);
#7207=ORIENTED_EDGE('',*,*,#5293,.F.);
#7208=ORIENTED_EDGE('',*,*,#5294,.T.);
#7209=ORIENTED_EDGE('',*,*,#5287,.F.);
#7210=ORIENTED_EDGE('',*,*,#5286,.F.);
#7211=ORIENTED_EDGE('',*,*,#5288,.F.);
#7212=ORIENTED_EDGE('',*,*,#5294,.F.);
#7213=ORIENTED_EDGE('',*,*,#5295,.F.);
#7214=ORIENTED_EDGE('',*,*,#5296,.T.);
#7215=ORIENTED_EDGE('',*,*,#5269,.T.);
#7216=ORIENTED_EDGE('',*,*,#5272,.T.);
#7217=ORIENTED_EDGE('',*,*,#5297,.T.);
#7218=ORIENTED_EDGE('',*,*,#5298,.F.);
#7219=ORIENTED_EDGE('',*,*,#5297,.F.);
#7220=ORIENTED_EDGE('',*,*,#5271,.T.);
#7221=ORIENTED_EDGE('',*,*,#5270,.T.);
#7222=ORIENTED_EDGE('',*,*,#5296,.F.);
#7223=ORIENTED_EDGE('',*,*,#5273,.T.);
#7224=ORIENTED_EDGE('',*,*,#5274,.T.);
#7225=ORIENTED_EDGE('',*,*,#5292,.T.);
#7226=ORIENTED_EDGE('',*,*,#5293,.T.);
#7227=ORIENTED_EDGE('',*,*,#5290,.T.);
#7228=ORIENTED_EDGE('',*,*,#5291,.T.);
#7229=ORIENTED_EDGE('',*,*,#5279,.T.);
#7230=ORIENTED_EDGE('',*,*,#5295,.T.);
#7231=ORIENTED_EDGE('',*,*,#5299,.T.);
#7232=ORIENTED_EDGE('',*,*,#5300,.T.);
#7233=ORIENTED_EDGE('',*,*,#5301,.F.);
#7234=ORIENTED_EDGE('',*,*,#5302,.T.);
#7235=ORIENTED_EDGE('',*,*,#5303,.F.);
#7236=ORIENTED_EDGE('',*,*,#5304,.T.);
#7237=ORIENTED_EDGE('',*,*,#5305,.F.);
#7238=ORIENTED_EDGE('',*,*,#5306,.T.);
#7239=ORIENTED_EDGE('',*,*,#5307,.F.);
#7240=ORIENTED_EDGE('',*,*,#5308,.T.);
#7241=ORIENTED_EDGE('',*,*,#5309,.F.);
#7242=ORIENTED_EDGE('',*,*,#5310,.T.);
#7243=ORIENTED_EDGE('',*,*,#5311,.F.);
#7244=ORIENTED_EDGE('',*,*,#5312,.T.);
#7245=ORIENTED_EDGE('',*,*,#5313,.F.);
#7246=ORIENTED_EDGE('',*,*,#5314,.T.);
#7247=ORIENTED_EDGE('',*,*,#5315,.F.);
#7248=ORIENTED_EDGE('',*,*,#5316,.T.);
#7249=ORIENTED_EDGE('',*,*,#5317,.F.);
#7250=ORIENTED_EDGE('',*,*,#5318,.T.);
#7251=ORIENTED_EDGE('',*,*,#5319,.F.);
#7252=ORIENTED_EDGE('',*,*,#5320,.T.);
#7253=ORIENTED_EDGE('',*,*,#5321,.F.);
#7254=ORIENTED_EDGE('',*,*,#5322,.T.);
#7255=ORIENTED_EDGE('',*,*,#5323,.F.);
#7256=ORIENTED_EDGE('',*,*,#5324,.T.);
#7257=ORIENTED_EDGE('',*,*,#5325,.F.);
#7258=ORIENTED_EDGE('',*,*,#5326,.T.);
#7259=ORIENTED_EDGE('',*,*,#5327,.F.);
#7260=ORIENTED_EDGE('',*,*,#5328,.T.);
#7261=ORIENTED_EDGE('',*,*,#5329,.F.);
#7262=ORIENTED_EDGE('',*,*,#5330,.T.);
#7263=ORIENTED_EDGE('',*,*,#5331,.F.);
#7264=ORIENTED_EDGE('',*,*,#5332,.T.);
#7265=ORIENTED_EDGE('',*,*,#5333,.F.);
#7266=ORIENTED_EDGE('',*,*,#5334,.T.);
#7267=ORIENTED_EDGE('',*,*,#5335,.F.);
#7268=ORIENTED_EDGE('',*,*,#5336,.T.);
#7269=ORIENTED_EDGE('',*,*,#5337,.F.);
#7270=ORIENTED_EDGE('',*,*,#5338,.T.);
#7271=ORIENTED_EDGE('',*,*,#5339,.F.);
#7272=ORIENTED_EDGE('',*,*,#5340,.F.);
#7273=ORIENTED_EDGE('',*,*,#5341,.T.);
#7274=ORIENTED_EDGE('',*,*,#5299,.F.);
#7275=ORIENTED_EDGE('',*,*,#5341,.F.);
#7276=ORIENTED_EDGE('',*,*,#5340,.T.);
#7277=ORIENTED_EDGE('',*,*,#5282,.T.);
#7278=ORIENTED_EDGE('',*,*,#5342,.F.);
#7279=ORIENTED_EDGE('',*,*,#5343,.T.);
#7280=ORIENTED_EDGE('',*,*,#5344,.T.);
#7281=ORIENTED_EDGE('',*,*,#5345,.T.);
#7282=ORIENTED_EDGE('',*,*,#5346,.T.);
#7283=ORIENTED_EDGE('',*,*,#5347,.T.);
#7284=ORIENTED_EDGE('',*,*,#5348,.T.);
#7285=ORIENTED_EDGE('',*,*,#5349,.T.);
#7286=ORIENTED_EDGE('',*,*,#5350,.T.);
#7287=ORIENTED_EDGE('',*,*,#5351,.T.);
#7288=ORIENTED_EDGE('',*,*,#5352,.T.);
#7289=ORIENTED_EDGE('',*,*,#5353,.T.);
#7290=ORIENTED_EDGE('',*,*,#5354,.T.);
#7291=ORIENTED_EDGE('',*,*,#5355,.T.);
#7292=ORIENTED_EDGE('',*,*,#5356,.T.);
#7293=ORIENTED_EDGE('',*,*,#5357,.T.);
#7294=ORIENTED_EDGE('',*,*,#5358,.T.);
#7295=ORIENTED_EDGE('',*,*,#5359,.T.);
#7296=ORIENTED_EDGE('',*,*,#5360,.T.);
#7297=ORIENTED_EDGE('',*,*,#5361,.T.);
#7298=ORIENTED_EDGE('',*,*,#5362,.T.);
#7299=ORIENTED_EDGE('',*,*,#5363,.T.);
#7300=ORIENTED_EDGE('',*,*,#5364,.T.);
#7301=ORIENTED_EDGE('',*,*,#5365,.T.);
#7302=ORIENTED_EDGE('',*,*,#5366,.T.);
#7303=ORIENTED_EDGE('',*,*,#5367,.T.);
#7304=ORIENTED_EDGE('',*,*,#5368,.T.);
#7305=ORIENTED_EDGE('',*,*,#5369,.T.);
#7306=ORIENTED_EDGE('',*,*,#5370,.T.);
#7307=ORIENTED_EDGE('',*,*,#5371,.T.);
#7308=ORIENTED_EDGE('',*,*,#5372,.T.);
#7309=ORIENTED_EDGE('',*,*,#5373,.T.);
#7310=ORIENTED_EDGE('',*,*,#5374,.T.);
#7311=ORIENTED_EDGE('',*,*,#5375,.T.);
#7312=ORIENTED_EDGE('',*,*,#5376,.T.);
#7313=ORIENTED_EDGE('',*,*,#5377,.T.);
#7314=ORIENTED_EDGE('',*,*,#5378,.T.);
#7315=ORIENTED_EDGE('',*,*,#5379,.T.);
#7316=ORIENTED_EDGE('',*,*,#5380,.T.);
#7317=ORIENTED_EDGE('',*,*,#5381,.T.);
#7318=ORIENTED_EDGE('',*,*,#5382,.T.);
#7319=ORIENTED_EDGE('',*,*,#5383,.F.);
#7320=ORIENTED_EDGE('',*,*,#5384,.T.);
#7321=ORIENTED_EDGE('',*,*,#5342,.T.);
#7322=ORIENTED_EDGE('',*,*,#5384,.F.);
#7323=ORIENTED_EDGE('',*,*,#5383,.T.);
#7324=ORIENTED_EDGE('',*,*,#5298,.T.);
#7325=ORIENTED_EDGE('',*,*,#5385,.F.);
#7326=ORIENTED_EDGE('',*,*,#5343,.F.);
#7327=ORIENTED_EDGE('',*,*,#5386,.F.);
#7328=ORIENTED_EDGE('',*,*,#5300,.F.);
#7329=ORIENTED_EDGE('',*,*,#5386,.T.);
#7330=ORIENTED_EDGE('',*,*,#5382,.F.);
#7331=ORIENTED_EDGE('',*,*,#5387,.T.);
#7332=ORIENTED_EDGE('',*,*,#5301,.T.);
#7333=ORIENTED_EDGE('',*,*,#5387,.F.);
#7334=ORIENTED_EDGE('',*,*,#5381,.F.);
#7335=ORIENTED_EDGE('',*,*,#5388,.F.);
#7336=ORIENTED_EDGE('',*,*,#5302,.F.);
#7337=ORIENTED_EDGE('',*,*,#5388,.T.);
#7338=ORIENTED_EDGE('',*,*,#5380,.F.);
#7339=ORIENTED_EDGE('',*,*,#5389,.T.);
#7340=ORIENTED_EDGE('',*,*,#5303,.T.);
#7341=ORIENTED_EDGE('',*,*,#5389,.F.);
#7342=ORIENTED_EDGE('',*,*,#5379,.F.);
#7343=ORIENTED_EDGE('',*,*,#5390,.F.);
#7344=ORIENTED_EDGE('',*,*,#5304,.F.);
#7345=ORIENTED_EDGE('',*,*,#5390,.T.);
#7346=ORIENTED_EDGE('',*,*,#5378,.F.);
#7347=ORIENTED_EDGE('',*,*,#5391,.T.);
#7348=ORIENTED_EDGE('',*,*,#5305,.T.);
#7349=ORIENTED_EDGE('',*,*,#5391,.F.);
#7350=ORIENTED_EDGE('',*,*,#5377,.F.);
#7351=ORIENTED_EDGE('',*,*,#5392,.F.);
#7352=ORIENTED_EDGE('',*,*,#5306,.F.);
#7353=ORIENTED_EDGE('',*,*,#5392,.T.);
#7354=ORIENTED_EDGE('',*,*,#5376,.F.);
#7355=ORIENTED_EDGE('',*,*,#5393,.T.);
#7356=ORIENTED_EDGE('',*,*,#5307,.T.);
#7357=ORIENTED_EDGE('',*,*,#5393,.F.);
#7358=ORIENTED_EDGE('',*,*,#5375,.F.);
#7359=ORIENTED_EDGE('',*,*,#5394,.F.);
#7360=ORIENTED_EDGE('',*,*,#5308,.F.);
#7361=ORIENTED_EDGE('',*,*,#5394,.T.);
#7362=ORIENTED_EDGE('',*,*,#5374,.F.);
#7363=ORIENTED_EDGE('',*,*,#5395,.T.);
#7364=ORIENTED_EDGE('',*,*,#5309,.T.);
#7365=ORIENTED_EDGE('',*,*,#5395,.F.);
#7366=ORIENTED_EDGE('',*,*,#5373,.F.);
#7367=ORIENTED_EDGE('',*,*,#5396,.F.);
#7368=ORIENTED_EDGE('',*,*,#5310,.F.);
#7369=ORIENTED_EDGE('',*,*,#5396,.T.);
#7370=ORIENTED_EDGE('',*,*,#5372,.F.);
#7371=ORIENTED_EDGE('',*,*,#5397,.T.);
#7372=ORIENTED_EDGE('',*,*,#5311,.T.);
#7373=ORIENTED_EDGE('',*,*,#5397,.F.);
#7374=ORIENTED_EDGE('',*,*,#5371,.F.);
#7375=ORIENTED_EDGE('',*,*,#5398,.F.);
#7376=ORIENTED_EDGE('',*,*,#5312,.F.);
#7377=ORIENTED_EDGE('',*,*,#5398,.T.);
#7378=ORIENTED_EDGE('',*,*,#5370,.F.);
#7379=ORIENTED_EDGE('',*,*,#5399,.T.);
#7380=ORIENTED_EDGE('',*,*,#5313,.T.);
#7381=ORIENTED_EDGE('',*,*,#5399,.F.);
#7382=ORIENTED_EDGE('',*,*,#5369,.F.);
#7383=ORIENTED_EDGE('',*,*,#5400,.F.);
#7384=ORIENTED_EDGE('',*,*,#5314,.F.);
#7385=ORIENTED_EDGE('',*,*,#5400,.T.);
#7386=ORIENTED_EDGE('',*,*,#5368,.F.);
#7387=ORIENTED_EDGE('',*,*,#5401,.T.);
#7388=ORIENTED_EDGE('',*,*,#5315,.T.);
#7389=ORIENTED_EDGE('',*,*,#5401,.F.);
#7390=ORIENTED_EDGE('',*,*,#5367,.F.);
#7391=ORIENTED_EDGE('',*,*,#5402,.F.);
#7392=ORIENTED_EDGE('',*,*,#5316,.F.);
#7393=ORIENTED_EDGE('',*,*,#5402,.T.);
#7394=ORIENTED_EDGE('',*,*,#5366,.F.);
#7395=ORIENTED_EDGE('',*,*,#5403,.T.);
#7396=ORIENTED_EDGE('',*,*,#5317,.T.);
#7397=ORIENTED_EDGE('',*,*,#5403,.F.);
#7398=ORIENTED_EDGE('',*,*,#5365,.F.);
#7399=ORIENTED_EDGE('',*,*,#5404,.F.);
#7400=ORIENTED_EDGE('',*,*,#5318,.F.);
#7401=ORIENTED_EDGE('',*,*,#5404,.T.);
#7402=ORIENTED_EDGE('',*,*,#5364,.F.);
#7403=ORIENTED_EDGE('',*,*,#5405,.T.);
#7404=ORIENTED_EDGE('',*,*,#5319,.T.);
#7405=ORIENTED_EDGE('',*,*,#5405,.F.);
#7406=ORIENTED_EDGE('',*,*,#5363,.F.);
#7407=ORIENTED_EDGE('',*,*,#5406,.F.);
#7408=ORIENTED_EDGE('',*,*,#5320,.F.);
#7409=ORIENTED_EDGE('',*,*,#5406,.T.);
#7410=ORIENTED_EDGE('',*,*,#5362,.F.);
#7411=ORIENTED_EDGE('',*,*,#5407,.T.);
#7412=ORIENTED_EDGE('',*,*,#5321,.T.);
#7413=ORIENTED_EDGE('',*,*,#5407,.F.);
#7414=ORIENTED_EDGE('',*,*,#5361,.F.);
#7415=ORIENTED_EDGE('',*,*,#5408,.F.);
#7416=ORIENTED_EDGE('',*,*,#5322,.F.);
#7417=ORIENTED_EDGE('',*,*,#5408,.T.);
#7418=ORIENTED_EDGE('',*,*,#5360,.F.);
#7419=ORIENTED_EDGE('',*,*,#5409,.T.);
#7420=ORIENTED_EDGE('',*,*,#5323,.T.);
#7421=ORIENTED_EDGE('',*,*,#5409,.F.);
#7422=ORIENTED_EDGE('',*,*,#5359,.F.);
#7423=ORIENTED_EDGE('',*,*,#5410,.F.);
#7424=ORIENTED_EDGE('',*,*,#5324,.F.);
#7425=ORIENTED_EDGE('',*,*,#5410,.T.);
#7426=ORIENTED_EDGE('',*,*,#5358,.F.);
#7427=ORIENTED_EDGE('',*,*,#5411,.T.);
#7428=ORIENTED_EDGE('',*,*,#5325,.T.);
#7429=ORIENTED_EDGE('',*,*,#5411,.F.);
#7430=ORIENTED_EDGE('',*,*,#5357,.F.);
#7431=ORIENTED_EDGE('',*,*,#5412,.F.);
#7432=ORIENTED_EDGE('',*,*,#5326,.F.);
#7433=ORIENTED_EDGE('',*,*,#5412,.T.);
#7434=ORIENTED_EDGE('',*,*,#5356,.F.);
#7435=ORIENTED_EDGE('',*,*,#5413,.T.);
#7436=ORIENTED_EDGE('',*,*,#5327,.T.);
#7437=ORIENTED_EDGE('',*,*,#5413,.F.);
#7438=ORIENTED_EDGE('',*,*,#5355,.F.);
#7439=ORIENTED_EDGE('',*,*,#5414,.F.);
#7440=ORIENTED_EDGE('',*,*,#5328,.F.);
#7441=ORIENTED_EDGE('',*,*,#5414,.T.);
#7442=ORIENTED_EDGE('',*,*,#5354,.F.);
#7443=ORIENTED_EDGE('',*,*,#5415,.T.);
#7444=ORIENTED_EDGE('',*,*,#5329,.T.);
#7445=ORIENTED_EDGE('',*,*,#5415,.F.);
#7446=ORIENTED_EDGE('',*,*,#5353,.F.);
#7447=ORIENTED_EDGE('',*,*,#5416,.F.);
#7448=ORIENTED_EDGE('',*,*,#5330,.F.);
#7449=ORIENTED_EDGE('',*,*,#5416,.T.);
#7450=ORIENTED_EDGE('',*,*,#5352,.F.);
#7451=ORIENTED_EDGE('',*,*,#5417,.T.);
#7452=ORIENTED_EDGE('',*,*,#5331,.T.);
#7453=ORIENTED_EDGE('',*,*,#5417,.F.);
#7454=ORIENTED_EDGE('',*,*,#5351,.F.);
#7455=ORIENTED_EDGE('',*,*,#5418,.F.);
#7456=ORIENTED_EDGE('',*,*,#5332,.F.);
#7457=ORIENTED_EDGE('',*,*,#5418,.T.);
#7458=ORIENTED_EDGE('',*,*,#5350,.F.);
#7459=ORIENTED_EDGE('',*,*,#5419,.T.);
#7460=ORIENTED_EDGE('',*,*,#5333,.T.);
#7461=ORIENTED_EDGE('',*,*,#5419,.F.);
#7462=ORIENTED_EDGE('',*,*,#5349,.F.);
#7463=ORIENTED_EDGE('',*,*,#5420,.F.);
#7464=ORIENTED_EDGE('',*,*,#5334,.F.);
#7465=ORIENTED_EDGE('',*,*,#5420,.T.);
#7466=ORIENTED_EDGE('',*,*,#5348,.F.);
#7467=ORIENTED_EDGE('',*,*,#5421,.T.);
#7468=ORIENTED_EDGE('',*,*,#5335,.T.);
#7469=ORIENTED_EDGE('',*,*,#5422,.F.);
#7470=ORIENTED_EDGE('',*,*,#5336,.F.);
#7471=ORIENTED_EDGE('',*,*,#5421,.F.);
#7472=ORIENTED_EDGE('',*,*,#5347,.F.);
#7473=ORIENTED_EDGE('',*,*,#5385,.T.);
#7474=ORIENTED_EDGE('',*,*,#5339,.T.);
#7475=ORIENTED_EDGE('',*,*,#5423,.T.);
#7476=ORIENTED_EDGE('',*,*,#5344,.F.);
#7477=ORIENTED_EDGE('',*,*,#5424,.F.);
#7478=ORIENTED_EDGE('',*,*,#5345,.F.);
#7479=ORIENTED_EDGE('',*,*,#5423,.F.);
#7480=ORIENTED_EDGE('',*,*,#5338,.F.);
#7481=ORIENTED_EDGE('',*,*,#5422,.T.);
#7482=ORIENTED_EDGE('',*,*,#5346,.F.);
#7483=ORIENTED_EDGE('',*,*,#5424,.T.);
#7484=ORIENTED_EDGE('',*,*,#5337,.T.);
#7485=ORIENTED_EDGE('',*,*,#5425,.F.);
#7486=ORIENTED_EDGE('',*,*,#5426,.T.);
#7487=ORIENTED_EDGE('',*,*,#5427,.T.);
#7488=ORIENTED_EDGE('',*,*,#5426,.F.);
#7489=ORIENTED_EDGE('',*,*,#5427,.F.);
#7490=ORIENTED_EDGE('',*,*,#5428,.T.);
#7491=ORIENTED_EDGE('',*,*,#5429,.F.);
#7492=ORIENTED_EDGE('',*,*,#5430,.F.);
#7493=ORIENTED_EDGE('',*,*,#5431,.F.);
#7494=ORIENTED_EDGE('',*,*,#5428,.F.);
#7495=ORIENTED_EDGE('',*,*,#5432,.T.);
#7496=ORIENTED_EDGE('',*,*,#5430,.T.);
#7497=ORIENTED_EDGE('',*,*,#5432,.F.);
#7498=ORIENTED_EDGE('',*,*,#5431,.T.);
#7499=ORIENTED_EDGE('',*,*,#5433,.T.);
#7500=ORIENTED_EDGE('',*,*,#5434,.T.);
#7501=ORIENTED_EDGE('',*,*,#5433,.F.);
#7502=ORIENTED_EDGE('',*,*,#5434,.F.);
#7503=ORIENTED_EDGE('',*,*,#5425,.T.);
#7504=ORIENTED_EDGE('',*,*,#5435,.F.);
#7505=ORIENTED_EDGE('',*,*,#5436,.T.);
#7506=ORIENTED_EDGE('',*,*,#5429,.T.);
#7507=ORIENTED_EDGE('',*,*,#5436,.F.);
#7508=ORIENTED_EDGE('',*,*,#5435,.T.);
#7509=ORIENTED_EDGE('',*,*,#5437,.F.);
#7510=ORIENTED_EDGE('',*,*,#5438,.T.);
#7511=ORIENTED_EDGE('',*,*,#5439,.T.);
#7512=ORIENTED_EDGE('',*,*,#5438,.F.);
#7513=ORIENTED_EDGE('',*,*,#5440,.F.);
#7514=ORIENTED_EDGE('',*,*,#5441,.T.);
#7515=ORIENTED_EDGE('',*,*,#5442,.T.);
#7516=ORIENTED_EDGE('',*,*,#5441,.F.);
#7517=ORIENTED_EDGE('',*,*,#5440,.T.);
#7518=ORIENTED_EDGE('',*,*,#5437,.T.);
#7519=ORIENTED_EDGE('',*,*,#5442,.F.);
#7520=ORIENTED_EDGE('',*,*,#5439,.F.);
#7521=ORIENTED_EDGE('',*,*,#5443,.F.);
#7522=ORIENTED_EDGE('',*,*,#5444,.T.);
#7523=ORIENTED_EDGE('',*,*,#5445,.T.);
#7524=ORIENTED_EDGE('',*,*,#5444,.F.);
#7525=ORIENTED_EDGE('',*,*,#5446,.F.);
#7526=ORIENTED_EDGE('',*,*,#5447,.T.);
#7527=ORIENTED_EDGE('',*,*,#5448,.T.);
#7528=ORIENTED_EDGE('',*,*,#5447,.F.);
#7529=ORIENTED_EDGE('',*,*,#5446,.T.);
#7530=ORIENTED_EDGE('',*,*,#5443,.T.);
#7531=ORIENTED_EDGE('',*,*,#5448,.F.);
#7532=ORIENTED_EDGE('',*,*,#5445,.F.);
#7533=ORIENTED_EDGE('',*,*,#5449,.F.);
#7534=ORIENTED_EDGE('',*,*,#5450,.T.);
#7535=ORIENTED_EDGE('',*,*,#5451,.T.);
#7536=ORIENTED_EDGE('',*,*,#5450,.F.);
#7537=ORIENTED_EDGE('',*,*,#5449,.T.);
#7538=ORIENTED_EDGE('',*,*,#5451,.F.);
#7539=ORIENTED_EDGE('',*,*,#5452,.F.);
#7540=ORIENTED_EDGE('',*,*,#5453,.T.);
#7541=ORIENTED_EDGE('',*,*,#5454,.T.);
#7542=ORIENTED_EDGE('',*,*,#5453,.F.);
#7543=ORIENTED_EDGE('',*,*,#5452,.T.);
#7544=ORIENTED_EDGE('',*,*,#5454,.F.);
#7545=ORIENTED_EDGE('',*,*,#5455,.F.);
#7546=ORIENTED_EDGE('',*,*,#5456,.T.);
#7547=ORIENTED_EDGE('',*,*,#5457,.T.);
#7548=ORIENTED_EDGE('',*,*,#5456,.F.);
#7549=ORIENTED_EDGE('',*,*,#5458,.F.);
#7550=ORIENTED_EDGE('',*,*,#5459,.T.);
#7551=ORIENTED_EDGE('',*,*,#5460,.T.);
#7552=ORIENTED_EDGE('',*,*,#5459,.F.);
#7553=ORIENTED_EDGE('',*,*,#5458,.T.);
#7554=ORIENTED_EDGE('',*,*,#5455,.T.);
#7555=ORIENTED_EDGE('',*,*,#5460,.F.);
#7556=ORIENTED_EDGE('',*,*,#5457,.F.);
#7557=ORIENTED_EDGE('',*,*,#5461,.F.);
#7558=ORIENTED_EDGE('',*,*,#5462,.F.);
#7559=ORIENTED_EDGE('',*,*,#5463,.F.);
#7560=ORIENTED_EDGE('',*,*,#5464,.T.);
#7561=ORIENTED_EDGE('',*,*,#5465,.F.);
#7562=ORIENTED_EDGE('',*,*,#5466,.F.);
#7563=ORIENTED_EDGE('',*,*,#5467,.F.);
#7564=ORIENTED_EDGE('',*,*,#5468,.F.);
#7565=ORIENTED_EDGE('',*,*,#5464,.F.);
#7566=ORIENTED_EDGE('',*,*,#5469,.F.);
#7567=ORIENTED_EDGE('',*,*,#5470,.F.);
#7568=ORIENTED_EDGE('',*,*,#5471,.T.);
#7569=ORIENTED_EDGE('',*,*,#5472,.F.);
#7570=ORIENTED_EDGE('',*,*,#5473,.F.);
#7571=ORIENTED_EDGE('',*,*,#5474,.F.);
#7572=ORIENTED_EDGE('',*,*,#5471,.F.);
#7573=ORIENTED_EDGE('',*,*,#5475,.F.);
#7574=ORIENTED_EDGE('',*,*,#5476,.T.);
#7575=ORIENTED_EDGE('',*,*,#5462,.T.);
#7576=ORIENTED_EDGE('',*,*,#5477,.T.);
#7577=ORIENTED_EDGE('',*,*,#5478,.F.);
#7578=ORIENTED_EDGE('',*,*,#5477,.F.);
#7579=ORIENTED_EDGE('',*,*,#5461,.T.);
#7580=ORIENTED_EDGE('',*,*,#5463,.T.);
#7581=ORIENTED_EDGE('',*,*,#5476,.F.);
#7582=ORIENTED_EDGE('',*,*,#5473,.T.);
#7583=ORIENTED_EDGE('',*,*,#5472,.T.);
#7584=ORIENTED_EDGE('',*,*,#5474,.T.);
#7585=ORIENTED_EDGE('',*,*,#5479,.T.);
#7586=ORIENTED_EDGE('',*,*,#5480,.T.);
#7587=ORIENTED_EDGE('',*,*,#5481,.T.);
#7588=ORIENTED_EDGE('',*,*,#5482,.T.);
#7589=ORIENTED_EDGE('',*,*,#5483,.T.);
#7590=ORIENTED_EDGE('',*,*,#5484,.T.);
#7591=ORIENTED_EDGE('',*,*,#5480,.F.);
#7592=ORIENTED_EDGE('',*,*,#5479,.F.);
#7593=ORIENTED_EDGE('',*,*,#5481,.F.);
#7594=ORIENTED_EDGE('',*,*,#5485,.T.);
#7595=ORIENTED_EDGE('',*,*,#5486,.F.);
#7596=ORIENTED_EDGE('',*,*,#5487,.F.);
#7597=ORIENTED_EDGE('',*,*,#5485,.F.);
#7598=ORIENTED_EDGE('',*,*,#5488,.F.);
#7599=ORIENTED_EDGE('',*,*,#5489,.F.);
#7600=ORIENTED_EDGE('',*,*,#5490,.T.);
#7601=ORIENTED_EDGE('',*,*,#5483,.F.);
#7602=ORIENTED_EDGE('',*,*,#5482,.F.);
#7603=ORIENTED_EDGE('',*,*,#5484,.F.);
#7604=ORIENTED_EDGE('',*,*,#5490,.F.);
#7605=ORIENTED_EDGE('',*,*,#5491,.F.);
#7606=ORIENTED_EDGE('',*,*,#5492,.T.);
#7607=ORIENTED_EDGE('',*,*,#5465,.T.);
#7608=ORIENTED_EDGE('',*,*,#5468,.T.);
#7609=ORIENTED_EDGE('',*,*,#5493,.T.);
#7610=ORIENTED_EDGE('',*,*,#5494,.F.);
#7611=ORIENTED_EDGE('',*,*,#5493,.F.);
#7612=ORIENTED_EDGE('',*,*,#5467,.T.);
#7613=ORIENTED_EDGE('',*,*,#5466,.T.);
#7614=ORIENTED_EDGE('',*,*,#5492,.F.);
#7615=ORIENTED_EDGE('',*,*,#5469,.T.);
#7616=ORIENTED_EDGE('',*,*,#5470,.T.);
#7617=ORIENTED_EDGE('',*,*,#5488,.T.);
#7618=ORIENTED_EDGE('',*,*,#5489,.T.);
#7619=ORIENTED_EDGE('',*,*,#5486,.T.);
#7620=ORIENTED_EDGE('',*,*,#5487,.T.);
#7621=ORIENTED_EDGE('',*,*,#5475,.T.);
#7622=ORIENTED_EDGE('',*,*,#5491,.T.);
#7623=ORIENTED_EDGE('',*,*,#5495,.T.);
#7624=ORIENTED_EDGE('',*,*,#5496,.T.);
#7625=ORIENTED_EDGE('',*,*,#5497,.F.);
#7626=ORIENTED_EDGE('',*,*,#5498,.T.);
#7627=ORIENTED_EDGE('',*,*,#5499,.F.);
#7628=ORIENTED_EDGE('',*,*,#5500,.T.);
#7629=ORIENTED_EDGE('',*,*,#5501,.F.);
#7630=ORIENTED_EDGE('',*,*,#5502,.T.);
#7631=ORIENTED_EDGE('',*,*,#5503,.F.);
#7632=ORIENTED_EDGE('',*,*,#5504,.T.);
#7633=ORIENTED_EDGE('',*,*,#5505,.F.);
#7634=ORIENTED_EDGE('',*,*,#5506,.T.);
#7635=ORIENTED_EDGE('',*,*,#5507,.F.);
#7636=ORIENTED_EDGE('',*,*,#5508,.T.);
#7637=ORIENTED_EDGE('',*,*,#5509,.F.);
#7638=ORIENTED_EDGE('',*,*,#5510,.T.);
#7639=ORIENTED_EDGE('',*,*,#5511,.F.);
#7640=ORIENTED_EDGE('',*,*,#5512,.T.);
#7641=ORIENTED_EDGE('',*,*,#5513,.F.);
#7642=ORIENTED_EDGE('',*,*,#5514,.T.);
#7643=ORIENTED_EDGE('',*,*,#5515,.F.);
#7644=ORIENTED_EDGE('',*,*,#5516,.T.);
#7645=ORIENTED_EDGE('',*,*,#5517,.F.);
#7646=ORIENTED_EDGE('',*,*,#5518,.T.);
#7647=ORIENTED_EDGE('',*,*,#5519,.F.);
#7648=ORIENTED_EDGE('',*,*,#5520,.T.);
#7649=ORIENTED_EDGE('',*,*,#5521,.F.);
#7650=ORIENTED_EDGE('',*,*,#5522,.T.);
#7651=ORIENTED_EDGE('',*,*,#5523,.F.);
#7652=ORIENTED_EDGE('',*,*,#5524,.T.);
#7653=ORIENTED_EDGE('',*,*,#5525,.F.);
#7654=ORIENTED_EDGE('',*,*,#5526,.T.);
#7655=ORIENTED_EDGE('',*,*,#5527,.F.);
#7656=ORIENTED_EDGE('',*,*,#5528,.T.);
#7657=ORIENTED_EDGE('',*,*,#5529,.F.);
#7658=ORIENTED_EDGE('',*,*,#5530,.T.);
#7659=ORIENTED_EDGE('',*,*,#5531,.F.);
#7660=ORIENTED_EDGE('',*,*,#5532,.T.);
#7661=ORIENTED_EDGE('',*,*,#5533,.F.);
#7662=ORIENTED_EDGE('',*,*,#5534,.T.);
#7663=ORIENTED_EDGE('',*,*,#5535,.F.);
#7664=ORIENTED_EDGE('',*,*,#5536,.T.);
#7665=ORIENTED_EDGE('',*,*,#5537,.F.);
#7666=ORIENTED_EDGE('',*,*,#5538,.T.);
#7667=ORIENTED_EDGE('',*,*,#5539,.F.);
#7668=ORIENTED_EDGE('',*,*,#5540,.T.);
#7669=ORIENTED_EDGE('',*,*,#5541,.F.);
#7670=ORIENTED_EDGE('',*,*,#5542,.T.);
#7671=ORIENTED_EDGE('',*,*,#5543,.F.);
#7672=ORIENTED_EDGE('',*,*,#5544,.T.);
#7673=ORIENTED_EDGE('',*,*,#5545,.F.);
#7674=ORIENTED_EDGE('',*,*,#5546,.T.);
#7675=ORIENTED_EDGE('',*,*,#5547,.F.);
#7676=ORIENTED_EDGE('',*,*,#5548,.T.);
#7677=ORIENTED_EDGE('',*,*,#5549,.F.);
#7678=ORIENTED_EDGE('',*,*,#5550,.T.);
#7679=ORIENTED_EDGE('',*,*,#5551,.F.);
#7680=ORIENTED_EDGE('',*,*,#5552,.T.);
#7681=ORIENTED_EDGE('',*,*,#5553,.F.);
#7682=ORIENTED_EDGE('',*,*,#5554,.T.);
#7683=ORIENTED_EDGE('',*,*,#5555,.F.);
#7684=ORIENTED_EDGE('',*,*,#5556,.T.);
#7685=ORIENTED_EDGE('',*,*,#5557,.F.);
#7686=ORIENTED_EDGE('',*,*,#5558,.T.);
#7687=ORIENTED_EDGE('',*,*,#5559,.F.);
#7688=ORIENTED_EDGE('',*,*,#5560,.T.);
#7689=ORIENTED_EDGE('',*,*,#5561,.F.);
#7690=ORIENTED_EDGE('',*,*,#5562,.T.);
#7691=ORIENTED_EDGE('',*,*,#5563,.F.);
#7692=ORIENTED_EDGE('',*,*,#5564,.T.);
#7693=ORIENTED_EDGE('',*,*,#5565,.F.);
#7694=ORIENTED_EDGE('',*,*,#5566,.T.);
#7695=ORIENTED_EDGE('',*,*,#5567,.F.);
#7696=ORIENTED_EDGE('',*,*,#5568,.T.);
#7697=ORIENTED_EDGE('',*,*,#5569,.F.);
#7698=ORIENTED_EDGE('',*,*,#5570,.T.);
#7699=ORIENTED_EDGE('',*,*,#5571,.F.);
#7700=ORIENTED_EDGE('',*,*,#5572,.T.);
#7701=ORIENTED_EDGE('',*,*,#5573,.F.);
#7702=ORIENTED_EDGE('',*,*,#5574,.T.);
#7703=ORIENTED_EDGE('',*,*,#5575,.F.);
#7704=ORIENTED_EDGE('',*,*,#5576,.F.);
#7705=ORIENTED_EDGE('',*,*,#5577,.T.);
#7706=ORIENTED_EDGE('',*,*,#5495,.F.);
#7707=ORIENTED_EDGE('',*,*,#5577,.F.);
#7708=ORIENTED_EDGE('',*,*,#5576,.T.);
#7709=ORIENTED_EDGE('',*,*,#5478,.T.);
#7710=ORIENTED_EDGE('',*,*,#5578,.F.);
#7711=ORIENTED_EDGE('',*,*,#5579,.T.);
#7712=ORIENTED_EDGE('',*,*,#5580,.T.);
#7713=ORIENTED_EDGE('',*,*,#5581,.T.);
#7714=ORIENTED_EDGE('',*,*,#5582,.T.);
#7715=ORIENTED_EDGE('',*,*,#5583,.T.);
#7716=ORIENTED_EDGE('',*,*,#5584,.T.);
#7717=ORIENTED_EDGE('',*,*,#5585,.T.);
#7718=ORIENTED_EDGE('',*,*,#5586,.T.);
#7719=ORIENTED_EDGE('',*,*,#5587,.T.);
#7720=ORIENTED_EDGE('',*,*,#5588,.T.);
#7721=ORIENTED_EDGE('',*,*,#5589,.T.);
#7722=ORIENTED_EDGE('',*,*,#5590,.T.);
#7723=ORIENTED_EDGE('',*,*,#5591,.T.);
#7724=ORIENTED_EDGE('',*,*,#5592,.T.);
#7725=ORIENTED_EDGE('',*,*,#5593,.T.);
#7726=ORIENTED_EDGE('',*,*,#5594,.T.);
#7727=ORIENTED_EDGE('',*,*,#5595,.T.);
#7728=ORIENTED_EDGE('',*,*,#5596,.T.);
#7729=ORIENTED_EDGE('',*,*,#5597,.T.);
#7730=ORIENTED_EDGE('',*,*,#5598,.T.);
#7731=ORIENTED_EDGE('',*,*,#5599,.T.);
#7732=ORIENTED_EDGE('',*,*,#5600,.T.);
#7733=ORIENTED_EDGE('',*,*,#5601,.T.);
#7734=ORIENTED_EDGE('',*,*,#5602,.T.);
#7735=ORIENTED_EDGE('',*,*,#5603,.T.);
#7736=ORIENTED_EDGE('',*,*,#5604,.T.);
#7737=ORIENTED_EDGE('',*,*,#5605,.T.);
#7738=ORIENTED_EDGE('',*,*,#5606,.T.);
#7739=ORIENTED_EDGE('',*,*,#5607,.T.);
#7740=ORIENTED_EDGE('',*,*,#5608,.T.);
#7741=ORIENTED_EDGE('',*,*,#5609,.T.);
#7742=ORIENTED_EDGE('',*,*,#5610,.T.);
#7743=ORIENTED_EDGE('',*,*,#5611,.T.);
#7744=ORIENTED_EDGE('',*,*,#5612,.T.);
#7745=ORIENTED_EDGE('',*,*,#5613,.T.);
#7746=ORIENTED_EDGE('',*,*,#5614,.T.);
#7747=ORIENTED_EDGE('',*,*,#5615,.T.);
#7748=ORIENTED_EDGE('',*,*,#5616,.T.);
#7749=ORIENTED_EDGE('',*,*,#5617,.T.);
#7750=ORIENTED_EDGE('',*,*,#5618,.T.);
#7751=ORIENTED_EDGE('',*,*,#5619,.T.);
#7752=ORIENTED_EDGE('',*,*,#5620,.T.);
#7753=ORIENTED_EDGE('',*,*,#5621,.T.);
#7754=ORIENTED_EDGE('',*,*,#5622,.T.);
#7755=ORIENTED_EDGE('',*,*,#5623,.T.);
#7756=ORIENTED_EDGE('',*,*,#5624,.T.);
#7757=ORIENTED_EDGE('',*,*,#5625,.T.);
#7758=ORIENTED_EDGE('',*,*,#5626,.T.);
#7759=ORIENTED_EDGE('',*,*,#5627,.T.);
#7760=ORIENTED_EDGE('',*,*,#5628,.T.);
#7761=ORIENTED_EDGE('',*,*,#5629,.T.);
#7762=ORIENTED_EDGE('',*,*,#5630,.T.);
#7763=ORIENTED_EDGE('',*,*,#5631,.T.);
#7764=ORIENTED_EDGE('',*,*,#5632,.T.);
#7765=ORIENTED_EDGE('',*,*,#5633,.T.);
#7766=ORIENTED_EDGE('',*,*,#5634,.T.);
#7767=ORIENTED_EDGE('',*,*,#5635,.T.);
#7768=ORIENTED_EDGE('',*,*,#5636,.T.);
#7769=ORIENTED_EDGE('',*,*,#5637,.T.);
#7770=ORIENTED_EDGE('',*,*,#5638,.T.);
#7771=ORIENTED_EDGE('',*,*,#5639,.T.);
#7772=ORIENTED_EDGE('',*,*,#5640,.T.);
#7773=ORIENTED_EDGE('',*,*,#5641,.T.);
#7774=ORIENTED_EDGE('',*,*,#5642,.T.);
#7775=ORIENTED_EDGE('',*,*,#5643,.T.);
#7776=ORIENTED_EDGE('',*,*,#5644,.T.);
#7777=ORIENTED_EDGE('',*,*,#5645,.T.);
#7778=ORIENTED_EDGE('',*,*,#5646,.T.);
#7779=ORIENTED_EDGE('',*,*,#5647,.T.);
#7780=ORIENTED_EDGE('',*,*,#5648,.T.);
#7781=ORIENTED_EDGE('',*,*,#5649,.T.);
#7782=ORIENTED_EDGE('',*,*,#5650,.T.);
#7783=ORIENTED_EDGE('',*,*,#5651,.T.);
#7784=ORIENTED_EDGE('',*,*,#5652,.T.);
#7785=ORIENTED_EDGE('',*,*,#5653,.T.);
#7786=ORIENTED_EDGE('',*,*,#5654,.T.);
#7787=ORIENTED_EDGE('',*,*,#5655,.T.);
#7788=ORIENTED_EDGE('',*,*,#5656,.T.);
#7789=ORIENTED_EDGE('',*,*,#5657,.T.);
#7790=ORIENTED_EDGE('',*,*,#5658,.T.);
#7791=ORIENTED_EDGE('',*,*,#5659,.F.);
#7792=ORIENTED_EDGE('',*,*,#5660,.T.);
#7793=ORIENTED_EDGE('',*,*,#5578,.T.);
#7794=ORIENTED_EDGE('',*,*,#5660,.F.);
#7795=ORIENTED_EDGE('',*,*,#5659,.T.);
#7796=ORIENTED_EDGE('',*,*,#5494,.T.);
#7797=ORIENTED_EDGE('',*,*,#5661,.F.);
#7798=ORIENTED_EDGE('',*,*,#5579,.F.);
#7799=ORIENTED_EDGE('',*,*,#5662,.F.);
#7800=ORIENTED_EDGE('',*,*,#5496,.F.);
#7801=ORIENTED_EDGE('',*,*,#5662,.T.);
#7802=ORIENTED_EDGE('',*,*,#5658,.F.);
#7803=ORIENTED_EDGE('',*,*,#5663,.T.);
#7804=ORIENTED_EDGE('',*,*,#5497,.T.);
#7805=ORIENTED_EDGE('',*,*,#5663,.F.);
#7806=ORIENTED_EDGE('',*,*,#5657,.F.);
#7807=ORIENTED_EDGE('',*,*,#5664,.F.);
#7808=ORIENTED_EDGE('',*,*,#5498,.F.);
#7809=ORIENTED_EDGE('',*,*,#5664,.T.);
#7810=ORIENTED_EDGE('',*,*,#5656,.F.);
#7811=ORIENTED_EDGE('',*,*,#5665,.T.);
#7812=ORIENTED_EDGE('',*,*,#5499,.T.);
#7813=ORIENTED_EDGE('',*,*,#5665,.F.);
#7814=ORIENTED_EDGE('',*,*,#5655,.F.);
#7815=ORIENTED_EDGE('',*,*,#5666,.F.);
#7816=ORIENTED_EDGE('',*,*,#5500,.F.);
#7817=ORIENTED_EDGE('',*,*,#5666,.T.);
#7818=ORIENTED_EDGE('',*,*,#5654,.F.);
#7819=ORIENTED_EDGE('',*,*,#5667,.T.);
#7820=ORIENTED_EDGE('',*,*,#5501,.T.);
#7821=ORIENTED_EDGE('',*,*,#5667,.F.);
#7822=ORIENTED_EDGE('',*,*,#5653,.F.);
#7823=ORIENTED_EDGE('',*,*,#5668,.F.);
#7824=ORIENTED_EDGE('',*,*,#5502,.F.);
#7825=ORIENTED_EDGE('',*,*,#5668,.T.);
#7826=ORIENTED_EDGE('',*,*,#5652,.F.);
#7827=ORIENTED_EDGE('',*,*,#5669,.T.);
#7828=ORIENTED_EDGE('',*,*,#5503,.T.);
#7829=ORIENTED_EDGE('',*,*,#5669,.F.);
#7830=ORIENTED_EDGE('',*,*,#5651,.F.);
#7831=ORIENTED_EDGE('',*,*,#5670,.F.);
#7832=ORIENTED_EDGE('',*,*,#5504,.F.);
#7833=ORIENTED_EDGE('',*,*,#5670,.T.);
#7834=ORIENTED_EDGE('',*,*,#5650,.F.);
#7835=ORIENTED_EDGE('',*,*,#5671,.T.);
#7836=ORIENTED_EDGE('',*,*,#5505,.T.);
#7837=ORIENTED_EDGE('',*,*,#5671,.F.);
#7838=ORIENTED_EDGE('',*,*,#5649,.F.);
#7839=ORIENTED_EDGE('',*,*,#5672,.F.);
#7840=ORIENTED_EDGE('',*,*,#5506,.F.);
#7841=ORIENTED_EDGE('',*,*,#5672,.T.);
#7842=ORIENTED_EDGE('',*,*,#5648,.F.);
#7843=ORIENTED_EDGE('',*,*,#5673,.T.);
#7844=ORIENTED_EDGE('',*,*,#5507,.T.);
#7845=ORIENTED_EDGE('',*,*,#5673,.F.);
#7846=ORIENTED_EDGE('',*,*,#5647,.F.);
#7847=ORIENTED_EDGE('',*,*,#5674,.F.);
#7848=ORIENTED_EDGE('',*,*,#5508,.F.);
#7849=ORIENTED_EDGE('',*,*,#5674,.T.);
#7850=ORIENTED_EDGE('',*,*,#5646,.F.);
#7851=ORIENTED_EDGE('',*,*,#5675,.T.);
#7852=ORIENTED_EDGE('',*,*,#5509,.T.);
#7853=ORIENTED_EDGE('',*,*,#5675,.F.);
#7854=ORIENTED_EDGE('',*,*,#5645,.F.);
#7855=ORIENTED_EDGE('',*,*,#5676,.F.);
#7856=ORIENTED_EDGE('',*,*,#5510,.F.);
#7857=ORIENTED_EDGE('',*,*,#5676,.T.);
#7858=ORIENTED_EDGE('',*,*,#5644,.F.);
#7859=ORIENTED_EDGE('',*,*,#5677,.T.);
#7860=ORIENTED_EDGE('',*,*,#5511,.T.);
#7861=ORIENTED_EDGE('',*,*,#5677,.F.);
#7862=ORIENTED_EDGE('',*,*,#5643,.F.);
#7863=ORIENTED_EDGE('',*,*,#5678,.F.);
#7864=ORIENTED_EDGE('',*,*,#5512,.F.);
#7865=ORIENTED_EDGE('',*,*,#5678,.T.);
#7866=ORIENTED_EDGE('',*,*,#5642,.F.);
#7867=ORIENTED_EDGE('',*,*,#5679,.T.);
#7868=ORIENTED_EDGE('',*,*,#5513,.T.);
#7869=ORIENTED_EDGE('',*,*,#5679,.F.);
#7870=ORIENTED_EDGE('',*,*,#5641,.F.);
#7871=ORIENTED_EDGE('',*,*,#5680,.F.);
#7872=ORIENTED_EDGE('',*,*,#5514,.F.);
#7873=ORIENTED_EDGE('',*,*,#5680,.T.);
#7874=ORIENTED_EDGE('',*,*,#5640,.F.);
#7875=ORIENTED_EDGE('',*,*,#5681,.T.);
#7876=ORIENTED_EDGE('',*,*,#5515,.T.);
#7877=ORIENTED_EDGE('',*,*,#5681,.F.);
#7878=ORIENTED_EDGE('',*,*,#5639,.F.);
#7879=ORIENTED_EDGE('',*,*,#5682,.F.);
#7880=ORIENTED_EDGE('',*,*,#5516,.F.);
#7881=ORIENTED_EDGE('',*,*,#5682,.T.);
#7882=ORIENTED_EDGE('',*,*,#5638,.F.);
#7883=ORIENTED_EDGE('',*,*,#5683,.T.);
#7884=ORIENTED_EDGE('',*,*,#5517,.T.);
#7885=ORIENTED_EDGE('',*,*,#5683,.F.);
#7886=ORIENTED_EDGE('',*,*,#5637,.F.);
#7887=ORIENTED_EDGE('',*,*,#5684,.F.);
#7888=ORIENTED_EDGE('',*,*,#5518,.F.);
#7889=ORIENTED_EDGE('',*,*,#5684,.T.);
#7890=ORIENTED_EDGE('',*,*,#5636,.F.);
#7891=ORIENTED_EDGE('',*,*,#5685,.T.);
#7892=ORIENTED_EDGE('',*,*,#5519,.T.);
#7893=ORIENTED_EDGE('',*,*,#5685,.F.);
#7894=ORIENTED_EDGE('',*,*,#5635,.F.);
#7895=ORIENTED_EDGE('',*,*,#5686,.F.);
#7896=ORIENTED_EDGE('',*,*,#5520,.F.);
#7897=ORIENTED_EDGE('',*,*,#5686,.T.);
#7898=ORIENTED_EDGE('',*,*,#5634,.F.);
#7899=ORIENTED_EDGE('',*,*,#5687,.T.);
#7900=ORIENTED_EDGE('',*,*,#5521,.T.);
#7901=ORIENTED_EDGE('',*,*,#5687,.F.);
#7902=ORIENTED_EDGE('',*,*,#5633,.F.);
#7903=ORIENTED_EDGE('',*,*,#5688,.F.);
#7904=ORIENTED_EDGE('',*,*,#5522,.F.);
#7905=ORIENTED_EDGE('',*,*,#5688,.T.);
#7906=ORIENTED_EDGE('',*,*,#5632,.F.);
#7907=ORIENTED_EDGE('',*,*,#5689,.T.);
#7908=ORIENTED_EDGE('',*,*,#5523,.T.);
#7909=ORIENTED_EDGE('',*,*,#5689,.F.);
#7910=ORIENTED_EDGE('',*,*,#5631,.F.);
#7911=ORIENTED_EDGE('',*,*,#5690,.F.);
#7912=ORIENTED_EDGE('',*,*,#5524,.F.);
#7913=ORIENTED_EDGE('',*,*,#5690,.T.);
#7914=ORIENTED_EDGE('',*,*,#5630,.F.);
#7915=ORIENTED_EDGE('',*,*,#5691,.T.);
#7916=ORIENTED_EDGE('',*,*,#5525,.T.);
#7917=ORIENTED_EDGE('',*,*,#5691,.F.);
#7918=ORIENTED_EDGE('',*,*,#5629,.F.);
#7919=ORIENTED_EDGE('',*,*,#5692,.F.);
#7920=ORIENTED_EDGE('',*,*,#5526,.F.);
#7921=ORIENTED_EDGE('',*,*,#5692,.T.);
#7922=ORIENTED_EDGE('',*,*,#5628,.F.);
#7923=ORIENTED_EDGE('',*,*,#5693,.T.);
#7924=ORIENTED_EDGE('',*,*,#5527,.T.);
#7925=ORIENTED_EDGE('',*,*,#5693,.F.);
#7926=ORIENTED_EDGE('',*,*,#5627,.F.);
#7927=ORIENTED_EDGE('',*,*,#5694,.F.);
#7928=ORIENTED_EDGE('',*,*,#5528,.F.);
#7929=ORIENTED_EDGE('',*,*,#5694,.T.);
#7930=ORIENTED_EDGE('',*,*,#5626,.F.);
#7931=ORIENTED_EDGE('',*,*,#5695,.T.);
#7932=ORIENTED_EDGE('',*,*,#5529,.T.);
#7933=ORIENTED_EDGE('',*,*,#5695,.F.);
#7934=ORIENTED_EDGE('',*,*,#5625,.F.);
#7935=ORIENTED_EDGE('',*,*,#5696,.F.);
#7936=ORIENTED_EDGE('',*,*,#5530,.F.);
#7937=ORIENTED_EDGE('',*,*,#5696,.T.);
#7938=ORIENTED_EDGE('',*,*,#5624,.F.);
#7939=ORIENTED_EDGE('',*,*,#5697,.T.);
#7940=ORIENTED_EDGE('',*,*,#5531,.T.);
#7941=ORIENTED_EDGE('',*,*,#5697,.F.);
#7942=ORIENTED_EDGE('',*,*,#5623,.F.);
#7943=ORIENTED_EDGE('',*,*,#5698,.F.);
#7944=ORIENTED_EDGE('',*,*,#5532,.F.);
#7945=ORIENTED_EDGE('',*,*,#5698,.T.);
#7946=ORIENTED_EDGE('',*,*,#5622,.F.);
#7947=ORIENTED_EDGE('',*,*,#5699,.T.);
#7948=ORIENTED_EDGE('',*,*,#5533,.T.);
#7949=ORIENTED_EDGE('',*,*,#5699,.F.);
#7950=ORIENTED_EDGE('',*,*,#5621,.F.);
#7951=ORIENTED_EDGE('',*,*,#5700,.F.);
#7952=ORIENTED_EDGE('',*,*,#5534,.F.);
#7953=ORIENTED_EDGE('',*,*,#5700,.T.);
#7954=ORIENTED_EDGE('',*,*,#5620,.F.);
#7955=ORIENTED_EDGE('',*,*,#5701,.T.);
#7956=ORIENTED_EDGE('',*,*,#5535,.T.);
#7957=ORIENTED_EDGE('',*,*,#5701,.F.);
#7958=ORIENTED_EDGE('',*,*,#5619,.F.);
#7959=ORIENTED_EDGE('',*,*,#5702,.F.);
#7960=ORIENTED_EDGE('',*,*,#5536,.F.);
#7961=ORIENTED_EDGE('',*,*,#5702,.T.);
#7962=ORIENTED_EDGE('',*,*,#5618,.F.);
#7963=ORIENTED_EDGE('',*,*,#5703,.T.);
#7964=ORIENTED_EDGE('',*,*,#5537,.T.);
#7965=ORIENTED_EDGE('',*,*,#5703,.F.);
#7966=ORIENTED_EDGE('',*,*,#5617,.F.);
#7967=ORIENTED_EDGE('',*,*,#5704,.F.);
#7968=ORIENTED_EDGE('',*,*,#5538,.F.);
#7969=ORIENTED_EDGE('',*,*,#5704,.T.);
#7970=ORIENTED_EDGE('',*,*,#5616,.F.);
#7971=ORIENTED_EDGE('',*,*,#5705,.T.);
#7972=ORIENTED_EDGE('',*,*,#5539,.T.);
#7973=ORIENTED_EDGE('',*,*,#5705,.F.);
#7974=ORIENTED_EDGE('',*,*,#5615,.F.);
#7975=ORIENTED_EDGE('',*,*,#5706,.F.);
#7976=ORIENTED_EDGE('',*,*,#5540,.F.);
#7977=ORIENTED_EDGE('',*,*,#5706,.T.);
#7978=ORIENTED_EDGE('',*,*,#5614,.F.);
#7979=ORIENTED_EDGE('',*,*,#5707,.T.);
#7980=ORIENTED_EDGE('',*,*,#5541,.T.);
#7981=ORIENTED_EDGE('',*,*,#5707,.F.);
#7982=ORIENTED_EDGE('',*,*,#5613,.F.);
#7983=ORIENTED_EDGE('',*,*,#5708,.F.);
#7984=ORIENTED_EDGE('',*,*,#5542,.F.);
#7985=ORIENTED_EDGE('',*,*,#5708,.T.);
#7986=ORIENTED_EDGE('',*,*,#5612,.F.);
#7987=ORIENTED_EDGE('',*,*,#5709,.T.);
#7988=ORIENTED_EDGE('',*,*,#5543,.T.);
#7989=ORIENTED_EDGE('',*,*,#5709,.F.);
#7990=ORIENTED_EDGE('',*,*,#5611,.F.);
#7991=ORIENTED_EDGE('',*,*,#5710,.F.);
#7992=ORIENTED_EDGE('',*,*,#5544,.F.);
#7993=ORIENTED_EDGE('',*,*,#5710,.T.);
#7994=ORIENTED_EDGE('',*,*,#5610,.F.);
#7995=ORIENTED_EDGE('',*,*,#5711,.T.);
#7996=ORIENTED_EDGE('',*,*,#5545,.T.);
#7997=ORIENTED_EDGE('',*,*,#5711,.F.);
#7998=ORIENTED_EDGE('',*,*,#5609,.F.);
#7999=ORIENTED_EDGE('',*,*,#5712,.F.);
#8000=ORIENTED_EDGE('',*,*,#5546,.F.);
#8001=ORIENTED_EDGE('',*,*,#5712,.T.);
#8002=ORIENTED_EDGE('',*,*,#5608,.F.);
#8003=ORIENTED_EDGE('',*,*,#5713,.T.);
#8004=ORIENTED_EDGE('',*,*,#5547,.T.);
#8005=ORIENTED_EDGE('',*,*,#5713,.F.);
#8006=ORIENTED_EDGE('',*,*,#5607,.F.);
#8007=ORIENTED_EDGE('',*,*,#5714,.F.);
#8008=ORIENTED_EDGE('',*,*,#5548,.F.);
#8009=ORIENTED_EDGE('',*,*,#5714,.T.);
#8010=ORIENTED_EDGE('',*,*,#5606,.F.);
#8011=ORIENTED_EDGE('',*,*,#5715,.T.);
#8012=ORIENTED_EDGE('',*,*,#5549,.T.);
#8013=ORIENTED_EDGE('',*,*,#5715,.F.);
#8014=ORIENTED_EDGE('',*,*,#5605,.F.);
#8015=ORIENTED_EDGE('',*,*,#5716,.F.);
#8016=ORIENTED_EDGE('',*,*,#5550,.F.);
#8017=ORIENTED_EDGE('',*,*,#5716,.T.);
#8018=ORIENTED_EDGE('',*,*,#5604,.F.);
#8019=ORIENTED_EDGE('',*,*,#5717,.T.);
#8020=ORIENTED_EDGE('',*,*,#5551,.T.);
#8021=ORIENTED_EDGE('',*,*,#5717,.F.);
#8022=ORIENTED_EDGE('',*,*,#5603,.F.);
#8023=ORIENTED_EDGE('',*,*,#5718,.F.);
#8024=ORIENTED_EDGE('',*,*,#5552,.F.);
#8025=ORIENTED_EDGE('',*,*,#5718,.T.);
#8026=ORIENTED_EDGE('',*,*,#5602,.F.);
#8027=ORIENTED_EDGE('',*,*,#5719,.T.);
#8028=ORIENTED_EDGE('',*,*,#5553,.T.);
#8029=ORIENTED_EDGE('',*,*,#5719,.F.);
#8030=ORIENTED_EDGE('',*,*,#5601,.F.);
#8031=ORIENTED_EDGE('',*,*,#5720,.F.);
#8032=ORIENTED_EDGE('',*,*,#5554,.F.);
#8033=ORIENTED_EDGE('',*,*,#5720,.T.);
#8034=ORIENTED_EDGE('',*,*,#5600,.F.);
#8035=ORIENTED_EDGE('',*,*,#5721,.T.);
#8036=ORIENTED_EDGE('',*,*,#5555,.T.);
#8037=ORIENTED_EDGE('',*,*,#5721,.F.);
#8038=ORIENTED_EDGE('',*,*,#5599,.F.);
#8039=ORIENTED_EDGE('',*,*,#5722,.F.);
#8040=ORIENTED_EDGE('',*,*,#5556,.F.);
#8041=ORIENTED_EDGE('',*,*,#5722,.T.);
#8042=ORIENTED_EDGE('',*,*,#5598,.F.);
#8043=ORIENTED_EDGE('',*,*,#5723,.T.);
#8044=ORIENTED_EDGE('',*,*,#5557,.T.);
#8045=ORIENTED_EDGE('',*,*,#5723,.F.);
#8046=ORIENTED_EDGE('',*,*,#5597,.F.);
#8047=ORIENTED_EDGE('',*,*,#5724,.F.);
#8048=ORIENTED_EDGE('',*,*,#5558,.F.);
#8049=ORIENTED_EDGE('',*,*,#5724,.T.);
#8050=ORIENTED_EDGE('',*,*,#5596,.F.);
#8051=ORIENTED_EDGE('',*,*,#5725,.T.);
#8052=ORIENTED_EDGE('',*,*,#5559,.T.);
#8053=ORIENTED_EDGE('',*,*,#5725,.F.);
#8054=ORIENTED_EDGE('',*,*,#5595,.F.);
#8055=ORIENTED_EDGE('',*,*,#5726,.F.);
#8056=ORIENTED_EDGE('',*,*,#5560,.F.);
#8057=ORIENTED_EDGE('',*,*,#5726,.T.);
#8058=ORIENTED_EDGE('',*,*,#5594,.F.);
#8059=ORIENTED_EDGE('',*,*,#5727,.T.);
#8060=ORIENTED_EDGE('',*,*,#5561,.T.);
#8061=ORIENTED_EDGE('',*,*,#5727,.F.);
#8062=ORIENTED_EDGE('',*,*,#5593,.F.);
#8063=ORIENTED_EDGE('',*,*,#5728,.F.);
#8064=ORIENTED_EDGE('',*,*,#5562,.F.);
#8065=ORIENTED_EDGE('',*,*,#5728,.T.);
#8066=ORIENTED_EDGE('',*,*,#5592,.F.);
#8067=ORIENTED_EDGE('',*,*,#5729,.T.);
#8068=ORIENTED_EDGE('',*,*,#5563,.T.);
#8069=ORIENTED_EDGE('',*,*,#5729,.F.);
#8070=ORIENTED_EDGE('',*,*,#5591,.F.);
#8071=ORIENTED_EDGE('',*,*,#5730,.F.);
#8072=ORIENTED_EDGE('',*,*,#5564,.F.);
#8073=ORIENTED_EDGE('',*,*,#5730,.T.);
#8074=ORIENTED_EDGE('',*,*,#5590,.F.);
#8075=ORIENTED_EDGE('',*,*,#5731,.T.);
#8076=ORIENTED_EDGE('',*,*,#5565,.T.);
#8077=ORIENTED_EDGE('',*,*,#5731,.F.);
#8078=ORIENTED_EDGE('',*,*,#5589,.F.);
#8079=ORIENTED_EDGE('',*,*,#5732,.F.);
#8080=ORIENTED_EDGE('',*,*,#5566,.F.);
#8081=ORIENTED_EDGE('',*,*,#5732,.T.);
#8082=ORIENTED_EDGE('',*,*,#5588,.F.);
#8083=ORIENTED_EDGE('',*,*,#5733,.T.);
#8084=ORIENTED_EDGE('',*,*,#5567,.T.);
#8085=ORIENTED_EDGE('',*,*,#5733,.F.);
#8086=ORIENTED_EDGE('',*,*,#5587,.F.);
#8087=ORIENTED_EDGE('',*,*,#5734,.F.);
#8088=ORIENTED_EDGE('',*,*,#5568,.F.);
#8089=ORIENTED_EDGE('',*,*,#5734,.T.);
#8090=ORIENTED_EDGE('',*,*,#5586,.F.);
#8091=ORIENTED_EDGE('',*,*,#5735,.T.);
#8092=ORIENTED_EDGE('',*,*,#5569,.T.);
#8093=ORIENTED_EDGE('',*,*,#5735,.F.);
#8094=ORIENTED_EDGE('',*,*,#5585,.F.);
#8095=ORIENTED_EDGE('',*,*,#5736,.F.);
#8096=ORIENTED_EDGE('',*,*,#5570,.F.);
#8097=ORIENTED_EDGE('',*,*,#5736,.T.);
#8098=ORIENTED_EDGE('',*,*,#5584,.F.);
#8099=ORIENTED_EDGE('',*,*,#5737,.T.);
#8100=ORIENTED_EDGE('',*,*,#5571,.T.);
#8101=ORIENTED_EDGE('',*,*,#5738,.F.);
#8102=ORIENTED_EDGE('',*,*,#5572,.F.);
#8103=ORIENTED_EDGE('',*,*,#5737,.F.);
#8104=ORIENTED_EDGE('',*,*,#5583,.F.);
#8105=ORIENTED_EDGE('',*,*,#5661,.T.);
#8106=ORIENTED_EDGE('',*,*,#5575,.T.);
#8107=ORIENTED_EDGE('',*,*,#5739,.T.);
#8108=ORIENTED_EDGE('',*,*,#5580,.F.);
#8109=ORIENTED_EDGE('',*,*,#5740,.F.);
#8110=ORIENTED_EDGE('',*,*,#5581,.F.);
#8111=ORIENTED_EDGE('',*,*,#5739,.F.);
#8112=ORIENTED_EDGE('',*,*,#5574,.F.);
#8113=ORIENTED_EDGE('',*,*,#5738,.T.);
#8114=ORIENTED_EDGE('',*,*,#5582,.F.);
#8115=ORIENTED_EDGE('',*,*,#5740,.T.);
#8116=ORIENTED_EDGE('',*,*,#5573,.T.);
#8117=ORIENTED_EDGE('',*,*,#5741,.F.);
#8118=ORIENTED_EDGE('',*,*,#5742,.F.);
#8119=ORIENTED_EDGE('',*,*,#5743,.T.);
#8120=ORIENTED_EDGE('',*,*,#5741,.T.);
#8121=ORIENTED_EDGE('',*,*,#5743,.F.);
#8122=ORIENTED_EDGE('',*,*,#5744,.F.);
#8123=ORIENTED_EDGE('',*,*,#5745,.T.);
#8124=ORIENTED_EDGE('',*,*,#5742,.T.);
#8125=ORIENTED_EDGE('',*,*,#5745,.F.);
#8126=ORIENTED_EDGE('',*,*,#5746,.F.);
#8127=ORIENTED_EDGE('',*,*,#5747,.T.);
#8128=ORIENTED_EDGE('',*,*,#5744,.T.);
#8129=ORIENTED_EDGE('',*,*,#5747,.F.);
#8130=ORIENTED_EDGE('',*,*,#5746,.T.);
#8131=ORIENTED_EDGE('',*,*,#5748,.F.);
#8132=ORIENTED_EDGE('',*,*,#5749,.F.);
#8133=ORIENTED_EDGE('',*,*,#5750,.T.);
#8134=ORIENTED_EDGE('',*,*,#5748,.T.);
#8135=ORIENTED_EDGE('',*,*,#5750,.F.);
#8136=ORIENTED_EDGE('',*,*,#5751,.F.);
#8137=ORIENTED_EDGE('',*,*,#5752,.T.);
#8138=ORIENTED_EDGE('',*,*,#5749,.T.);
#8139=ORIENTED_EDGE('',*,*,#5752,.F.);
#8140=ORIENTED_EDGE('',*,*,#5753,.F.);
#8141=ORIENTED_EDGE('',*,*,#5754,.T.);
#8142=ORIENTED_EDGE('',*,*,#5751,.T.);
#8143=ORIENTED_EDGE('',*,*,#5754,.F.);
#8144=ORIENTED_EDGE('',*,*,#5753,.T.);
#8145=ORIENTED_EDGE('',*,*,#5755,.T.);
#8146=ORIENTED_EDGE('',*,*,#5756,.T.);
#8147=ORIENTED_EDGE('',*,*,#5757,.T.);
#8148=ORIENTED_EDGE('',*,*,#5758,.F.);
#8149=ORIENTED_EDGE('',*,*,#5759,.T.);
#8150=ORIENTED_EDGE('',*,*,#5760,.T.);
#8151=ORIENTED_EDGE('',*,*,#5761,.T.);
#8152=ORIENTED_EDGE('',*,*,#5756,.F.);
#8153=ORIENTED_EDGE('',*,*,#5762,.T.);
#8154=ORIENTED_EDGE('',*,*,#5763,.T.);
#8155=ORIENTED_EDGE('',*,*,#5764,.T.);
#8156=ORIENTED_EDGE('',*,*,#5760,.F.);
#8157=ORIENTED_EDGE('',*,*,#5765,.T.);
#8158=ORIENTED_EDGE('',*,*,#5766,.T.);
#8159=ORIENTED_EDGE('',*,*,#5767,.T.);
#8160=ORIENTED_EDGE('',*,*,#5763,.F.);
#8161=ORIENTED_EDGE('',*,*,#5768,.T.);
#8162=ORIENTED_EDGE('',*,*,#5769,.T.);
#8163=ORIENTED_EDGE('',*,*,#5770,.T.);
#8164=ORIENTED_EDGE('',*,*,#5766,.F.);
#8165=ORIENTED_EDGE('',*,*,#5771,.T.);
#8166=ORIENTED_EDGE('',*,*,#5758,.T.);
#8167=ORIENTED_EDGE('',*,*,#5772,.T.);
#8168=ORIENTED_EDGE('',*,*,#5769,.F.);
#8169=ORIENTED_EDGE('',*,*,#5771,.F.);
#8170=ORIENTED_EDGE('',*,*,#5768,.F.);
#8171=ORIENTED_EDGE('',*,*,#5765,.F.);
#8172=ORIENTED_EDGE('',*,*,#5762,.F.);
#8173=ORIENTED_EDGE('',*,*,#5759,.F.);
#8174=ORIENTED_EDGE('',*,*,#5755,.F.);
#8175=ORIENTED_EDGE('',*,*,#5772,.F.);
#8176=ORIENTED_EDGE('',*,*,#5757,.F.);
#8177=ORIENTED_EDGE('',*,*,#5761,.F.);
#8178=ORIENTED_EDGE('',*,*,#5764,.F.);
#8179=ORIENTED_EDGE('',*,*,#5767,.F.);
#8180=ORIENTED_EDGE('',*,*,#5770,.F.);
#8181=CYLINDRICAL_SURFACE('',#9519,0.225);
#8182=CYLINDRICAL_SURFACE('',#9522,0.225);
#8183=CYLINDRICAL_SURFACE('',#9534,0.225);
#8184=CYLINDRICAL_SURFACE('',#9536,0.225);
#8185=CYLINDRICAL_SURFACE('',#9540,0.225);
#8186=CYLINDRICAL_SURFACE('',#9544,0.225);
#8187=CYLINDRICAL_SURFACE('',#9548,0.225);
#8188=CYLINDRICAL_SURFACE('',#9552,0.225);
#8189=CYLINDRICAL_SURFACE('',#9556,0.165);
#8190=CYLINDRICAL_SURFACE('',#9560,0.165);
#8191=CYLINDRICAL_SURFACE('',#9564,0.165);
#8192=CYLINDRICAL_SURFACE('',#9568,0.165);
#8193=CYLINDRICAL_SURFACE('',#9592,0.165);
#8194=CYLINDRICAL_SURFACE('',#9595,0.165);
#8195=CYLINDRICAL_SURFACE('',#9598,0.165);
#8196=CYLINDRICAL_SURFACE('',#9601,0.165);
#8197=CYLINDRICAL_SURFACE('',#9604,1.5);
#8198=CYLINDRICAL_SURFACE('',#9607,0.225);
#8199=CYLINDRICAL_SURFACE('',#9610,0.225);
#8200=CYLINDRICAL_SURFACE('',#9613,0.225);
#8201=CYLINDRICAL_SURFACE('',#9616,0.225);
#8202=CYLINDRICAL_SURFACE('',#9630,1.1);
#8203=CYLINDRICAL_SURFACE('',#9633,1.49);
#8204=CYLINDRICAL_SURFACE('',#9639,0.225);
#8205=CYLINDRICAL_SURFACE('',#9642,0.225);
#8206=CYLINDRICAL_SURFACE('',#9645,0.225);
#8207=CYLINDRICAL_SURFACE('',#9648,0.225);
#8208=CYLINDRICAL_SURFACE('',#9657,2.1);
#8209=CYLINDRICAL_SURFACE('',#9659,2.1);
#8210=CYLINDRICAL_SURFACE('',#9661,2.1);
#8211=CYLINDRICAL_SURFACE('',#9663,2.1);
#8212=CYLINDRICAL_SURFACE('',#9665,1.49);
#8213=CYLINDRICAL_SURFACE('',#9670,1.1);
#8214=CYLINDRICAL_SURFACE('',#9673,0.225);
#8215=CYLINDRICAL_SURFACE('',#9676,0.225);
#8216=CYLINDRICAL_SURFACE('',#9679,0.225);
#8217=CYLINDRICAL_SURFACE('',#9682,0.225);
#8218=CYLINDRICAL_SURFACE('',#9691,2.1);
#8219=CYLINDRICAL_SURFACE('',#9693,2.1);
#8220=CYLINDRICAL_SURFACE('',#9695,2.1);
#8221=CYLINDRICAL_SURFACE('',#9697,2.1);
#8222=CYLINDRICAL_SURFACE('',#9699,1.49);
#8223=CYLINDRICAL_SURFACE('',#9703,1.1);
#8224=CYLINDRICAL_SURFACE('',#9707,0.165);
#8225=CYLINDRICAL_SURFACE('',#9710,0.165);
#8226=CYLINDRICAL_SURFACE('',#9713,0.164999999999999);
#8227=CYLINDRICAL_SURFACE('',#9716,0.164999999999999);
#8228=CYLINDRICAL_SURFACE('',#9719,1.6);
#8229=CYLINDRICAL_SURFACE('',#9722,0.225);
#8230=CYLINDRICAL_SURFACE('',#9725,0.225);
#8231=CYLINDRICAL_SURFACE('',#9728,0.225);
#8232=CYLINDRICAL_SURFACE('',#9731,0.225);
#8233=CYLINDRICAL_SURFACE('',#9745,0.165);
#8234=CYLINDRICAL_SURFACE('',#9748,0.4);
#8235=CYLINDRICAL_SURFACE('',#9754,0.165);
#8236=CYLINDRICAL_SURFACE('',#9757,0.4);
#8237=CYLINDRICAL_SURFACE('',#9763,0.164999999999999);
#8238=CYLINDRICAL_SURFACE('',#9766,0.4);
#8239=CYLINDRICAL_SURFACE('',#9772,0.164999999999999);
#8240=CYLINDRICAL_SURFACE('',#9775,0.4);
#8241=CYLINDRICAL_SURFACE('',#9781,1.2);
#8242=CYLINDRICAL_SURFACE('',#9784,1.59);
#8243=CYLINDRICAL_SURFACE('',#9790,0.225);
#8244=CYLINDRICAL_SURFACE('',#9793,0.225);
#8245=CYLINDRICAL_SURFACE('',#9796,0.225);
#8246=CYLINDRICAL_SURFACE('',#9799,0.225);
#8247=CYLINDRICAL_SURFACE('',#9808,2.2);
#8248=CYLINDRICAL_SURFACE('',#9810,2.2);
#8249=CYLINDRICAL_SURFACE('',#9812,2.2);
#8250=CYLINDRICAL_SURFACE('',#9814,2.2);
#8251=CYLINDRICAL_SURFACE('',#9816,1.59);
#8252=CYLINDRICAL_SURFACE('',#9821,1.2);
#8253=CYLINDRICAL_SURFACE('',#9824,0.225);
#8254=CYLINDRICAL_SURFACE('',#9827,0.225);
#8255=CYLINDRICAL_SURFACE('',#9830,0.225);
#8256=CYLINDRICAL_SURFACE('',#9833,0.225);
#8257=CYLINDRICAL_SURFACE('',#9842,2.2);
#8258=CYLINDRICAL_SURFACE('',#9844,2.2);
#8259=CYLINDRICAL_SURFACE('',#9846,2.2);
#8260=CYLINDRICAL_SURFACE('',#9848,2.2);
#8261=CYLINDRICAL_SURFACE('',#9850,1.59);
#8262=CYLINDRICAL_SURFACE('',#9854,1.2);
#8263=CYLINDRICAL_SURFACE('',#9865,0.636619772367581);
#8264=CYLINDRICAL_SURFACE('',#9867,1.27323954473516);
#8265=CYLINDRICAL_SURFACE('',#9869,1.37323954473516);
#8266=CYLINDRICAL_SURFACE('',#9873,0.736619772367581);
#8267=CYLINDRICAL_SURFACE('',#9884,0.976185);
#8268=CYLINDRICAL_SURFACE('',#9886,0.5);
#8269=CYLINDRICAL_SURFACE('',#9892,0.976185);
#8270=CYLINDRICAL_SURFACE('',#9904,1.023815);
#8271=CYLINDRICAL_SURFACE('',#9911,1.5);
#8272=CYLINDRICAL_SURFACE('',#9916,1.023815);
#8273=CYLINDRICAL_SURFACE('',#9938,1.019052);
#8274=CYLINDRICAL_SURFACE('',#9978,0.980948);
#8275=CYLINDRICAL_SURFACE('',#9992,1.013815);
#8276=CYLINDRICAL_SURFACE('',#9996,0.991185);
#8277=CYLINDRICAL_SURFACE('',#10000,1.013815);
#8278=CYLINDRICAL_SURFACE('',#10004,0.991185);
#8279=CYLINDRICAL_SURFACE('',#10022,0.2);
#8280=CYLINDRICAL_SURFACE('',#10029,0.35);
#8281=CYLINDRICAL_SURFACE('',#10037,0.1954);
#8282=CYLINDRICAL_SURFACE('',#10048,1.070235);
#8283=CYLINDRICAL_SURFACE('',#10050,0.6);
#8284=CYLINDRICAL_SURFACE('',#10056,1.070235);
#8285=CYLINDRICAL_SURFACE('',#10068,1.129765);
#8286=CYLINDRICAL_SURFACE('',#10075,1.6);
#8287=CYLINDRICAL_SURFACE('',#10080,1.129765);
#8288=CYLINDRICAL_SURFACE('',#10100,1.123812);
#8289=CYLINDRICAL_SURFACE('',#10136,1.076188);
#8290=CYLINDRICAL_SURFACE('',#10150,1.119765);
#8291=CYLINDRICAL_SURFACE('',#10154,1.085235);
#8292=CYLINDRICAL_SURFACE('',#10158,1.119765);
#8293=CYLINDRICAL_SURFACE('',#10162,1.085235);
#8294=CYLINDRICAL_SURFACE('',#10183,0.35);
#8295=CYLINDRICAL_SURFACE('',#10191,0.1954);
#8296=CYLINDRICAL_SURFACE('',#10194,0.165);
#8297=CYLINDRICAL_SURFACE('',#10204,0.7);
#8298=CYLINDRICAL_SURFACE('',#10205,0.5);
#8299=CYLINDRICAL_SURFACE('',#10207,0.4);
#8300=CYLINDRICAL_SURFACE('',#10211,0.5);
#8301=CYLINDRICAL_SURFACE('',#10216,0.505);
#8302=CYLINDRICAL_SURFACE('',#10221,0.405);
#8303=CYLINDRICAL_SURFACE('',#10223,0.7);
#8304=CYLINDRICAL_SURFACE('',#10229,0.505);
#8305=CYLINDRICAL_SURFACE('',#10232,0.7);
#8306=CYLINDRICAL_SURFACE('',#10238,0.15);
#8307=CYLINDRICAL_SURFACE('',#10244,0.15);
#8308=CYLINDRICAL_SURFACE('',#10250,0.225);
#8309=CYLINDRICAL_SURFACE('',#10253,0.6);
#8310=CYLINDRICAL_SURFACE('',#10259,0.125);
#8311=CYLINDRICAL_SURFACE('',#10260,0.125);
#8312=CYLINDRICAL_SURFACE('',#10261,0.65);
#8313=CYLINDRICAL_SURFACE('',#10264,0.125);
#8314=CYLINDRICAL_SURFACE('',#10265,0.125);
#8315=CYLINDRICAL_SURFACE('',#10266,0.4);
#8316=CYLINDRICAL_SURFACE('',#10312,0.8);
#8317=CYLINDRICAL_SURFACE('',#10357,0.8);
#8318=CYLINDRICAL_SURFACE('',#10360,0.0555);
#8319=CYLINDRICAL_SURFACE('',#10361,0.611219772367581);
#8320=CYLINDRICAL_SURFACE('',#10362,0.0555);
#8321=CYLINDRICAL_SURFACE('',#10363,0.611219772367581);
#8322=CYLINDRICAL_SURFACE('',#10364,0.0555);
#8323=CYLINDRICAL_SURFACE('',#10365,0.611219772367581);
#8324=CYLINDRICAL_SURFACE('',#10366,0.0555);
#8325=CYLINDRICAL_SURFACE('',#10367,0.611219772367581);
#8326=CYLINDRICAL_SURFACE('',#10368,0.0555);
#8327=CYLINDRICAL_SURFACE('',#10369,0.611219772367581);
#8328=CYLINDRICAL_SURFACE('',#10370,0.0555);
#8329=CYLINDRICAL_SURFACE('',#10371,0.611219772367581);
#8330=CYLINDRICAL_SURFACE('',#10372,0.0555);
#8331=CYLINDRICAL_SURFACE('',#10373,0.611219772367581);
#8332=CYLINDRICAL_SURFACE('',#10374,0.0555);
#8333=CYLINDRICAL_SURFACE('',#10375,0.611219772367581);
#8334=CYLINDRICAL_SURFACE('',#10376,0.0555);
#8335=CYLINDRICAL_SURFACE('',#10377,0.611219772367581);
#8336=CYLINDRICAL_SURFACE('',#10378,0.0555);
#8337=CYLINDRICAL_SURFACE('',#10379,0.611219772367581);
#8338=CYLINDRICAL_SURFACE('',#10380,0.0555);
#8339=CYLINDRICAL_SURFACE('',#10381,0.611219772367581);
#8340=CYLINDRICAL_SURFACE('',#10382,0.0555);
#8341=CYLINDRICAL_SURFACE('',#10383,0.611219772367581);
#8342=CYLINDRICAL_SURFACE('',#10384,0.0555);
#8343=CYLINDRICAL_SURFACE('',#10385,0.611219772367581);
#8344=CYLINDRICAL_SURFACE('',#10386,0.0555);
#8345=CYLINDRICAL_SURFACE('',#10387,0.611219772367581);
#8346=CYLINDRICAL_SURFACE('',#10388,0.0555);
#8347=CYLINDRICAL_SURFACE('',#10389,0.611219772367581);
#8348=CYLINDRICAL_SURFACE('',#10390,0.0555);
#8349=CYLINDRICAL_SURFACE('',#10391,0.611219772367581);
#8350=CYLINDRICAL_SURFACE('',#10392,0.0555);
#8351=CYLINDRICAL_SURFACE('',#10393,0.611219772367581);
#8352=CYLINDRICAL_SURFACE('',#10394,0.0555);
#8353=CYLINDRICAL_SURFACE('',#10395,0.611219772367581);
#8354=CYLINDRICAL_SURFACE('',#10396,0.0555);
#8355=CYLINDRICAL_SURFACE('',#10397,0.611219772367581);
#8356=CYLINDRICAL_SURFACE('',#10398,0.0555);
#8357=CYLINDRICAL_SURFACE('',#10399,0.611219772367581);
#8358=CYLINDRICAL_SURFACE('',#10402,0.165);
#8359=CYLINDRICAL_SURFACE('',#10412,0.8);
#8360=CYLINDRICAL_SURFACE('',#10413,0.6);
#8361=CYLINDRICAL_SURFACE('',#10416,0.6);
#8362=CYLINDRICAL_SURFACE('',#10420,0.605);
#8363=CYLINDRICAL_SURFACE('',#10423,0.8);
#8364=CYLINDRICAL_SURFACE('',#10429,0.605);
#8365=CYLINDRICAL_SURFACE('',#10432,0.8);
#8366=CYLINDRICAL_SURFACE('',#10438,0.15);
#8367=CYLINDRICAL_SURFACE('',#10444,0.15);
#8368=CYLINDRICAL_SURFACE('',#10450,0.225);
#8369=CYLINDRICAL_SURFACE('',#10453,0.8);
#8370=CYLINDRICAL_SURFACE('',#10459,0.125);
#8371=CYLINDRICAL_SURFACE('',#10460,0.125);
#8372=CYLINDRICAL_SURFACE('',#10461,1.);
#8373=CYLINDRICAL_SURFACE('',#10464,0.125);
#8374=CYLINDRICAL_SURFACE('',#10465,0.125);
#8375=CYLINDRICAL_SURFACE('',#10466,0.6);
#8376=CYLINDRICAL_SURFACE('',#10552,1.4);
#8377=CYLINDRICAL_SURFACE('',#10637,1.4);
#8378=CYLINDRICAL_SURFACE('',#10640,0.0555000000000001);
#8379=CYLINDRICAL_SURFACE('',#10641,1.24783954473516);
#8380=CYLINDRICAL_SURFACE('',#10642,0.0555000000000001);
#8381=CYLINDRICAL_SURFACE('',#10643,1.24783954473516);
#8382=CYLINDRICAL_SURFACE('',#10644,0.0555000000000001);
#8383=CYLINDRICAL_SURFACE('',#10645,1.24783954473516);
#8384=CYLINDRICAL_SURFACE('',#10646,0.0555000000000001);
#8385=CYLINDRICAL_SURFACE('',#10647,1.24783954473516);
#8386=CYLINDRICAL_SURFACE('',#10648,0.0555000000000001);
#8387=CYLINDRICAL_SURFACE('',#10649,1.24783954473516);
#8388=CYLINDRICAL_SURFACE('',#10650,0.0555000000000001);
#8389=CYLINDRICAL_SURFACE('',#10651,1.24783954473516);
#8390=CYLINDRICAL_SURFACE('',#10652,0.0555000000000001);
#8391=CYLINDRICAL_SURFACE('',#10653,1.24783954473516);
#8392=CYLINDRICAL_SURFACE('',#10654,0.0555000000000001);
#8393=CYLINDRICAL_SURFACE('',#10655,1.24783954473516);
#8394=CYLINDRICAL_SURFACE('',#10656,0.0555000000000001);
#8395=CYLINDRICAL_SURFACE('',#10657,1.24783954473516);
#8396=CYLINDRICAL_SURFACE('',#10658,0.0555000000000001);
#8397=CYLINDRICAL_SURFACE('',#10659,1.24783954473516);
#8398=CYLINDRICAL_SURFACE('',#10660,0.0555000000000001);
#8399=CYLINDRICAL_SURFACE('',#10661,1.24783954473516);
#8400=CYLINDRICAL_SURFACE('',#10662,0.0555000000000001);
#8401=CYLINDRICAL_SURFACE('',#10663,1.24783954473516);
#8402=CYLINDRICAL_SURFACE('',#10664,0.0555000000000001);
#8403=CYLINDRICAL_SURFACE('',#10665,1.24783954473516);
#8404=CYLINDRICAL_SURFACE('',#10666,0.0555000000000001);
#8405=CYLINDRICAL_SURFACE('',#10667,1.24783954473516);
#8406=CYLINDRICAL_SURFACE('',#10668,0.0555000000000001);
#8407=CYLINDRICAL_SURFACE('',#10669,1.24783954473516);
#8408=CYLINDRICAL_SURFACE('',#10670,0.0555000000000001);
#8409=CYLINDRICAL_SURFACE('',#10671,1.24783954473516);
#8410=CYLINDRICAL_SURFACE('',#10672,0.0555000000000001);
#8411=CYLINDRICAL_SURFACE('',#10673,1.24783954473516);
#8412=CYLINDRICAL_SURFACE('',#10674,0.0555000000000001);
#8413=CYLINDRICAL_SURFACE('',#10675,1.24783954473516);
#8414=CYLINDRICAL_SURFACE('',#10676,0.0555000000000001);
#8415=CYLINDRICAL_SURFACE('',#10677,1.24783954473516);
#8416=CYLINDRICAL_SURFACE('',#10678,0.0555000000000001);
#8417=CYLINDRICAL_SURFACE('',#10679,1.24783954473516);
#8418=CYLINDRICAL_SURFACE('',#10680,0.0555000000000001);
#8419=CYLINDRICAL_SURFACE('',#10681,1.24783954473516);
#8420=CYLINDRICAL_SURFACE('',#10682,0.0555000000000001);
#8421=CYLINDRICAL_SURFACE('',#10683,1.24783954473516);
#8422=CYLINDRICAL_SURFACE('',#10684,0.0555000000000001);
#8423=CYLINDRICAL_SURFACE('',#10685,1.24783954473516);
#8424=CYLINDRICAL_SURFACE('',#10686,0.0555000000000001);
#8425=CYLINDRICAL_SURFACE('',#10687,1.24783954473516);
#8426=CYLINDRICAL_SURFACE('',#10688,0.0555000000000001);
#8427=CYLINDRICAL_SURFACE('',#10689,1.24783954473516);
#8428=CYLINDRICAL_SURFACE('',#10690,0.0555000000000001);
#8429=CYLINDRICAL_SURFACE('',#10691,1.24783954473516);
#8430=CYLINDRICAL_SURFACE('',#10692,0.0555000000000001);
#8431=CYLINDRICAL_SURFACE('',#10693,1.24783954473516);
#8432=CYLINDRICAL_SURFACE('',#10694,0.0555000000000001);
#8433=CYLINDRICAL_SURFACE('',#10695,1.24783954473516);
#8434=CYLINDRICAL_SURFACE('',#10696,0.0555000000000001);
#8435=CYLINDRICAL_SURFACE('',#10697,1.24783954473516);
#8436=CYLINDRICAL_SURFACE('',#10698,0.0555000000000001);
#8437=CYLINDRICAL_SURFACE('',#10699,1.24783954473516);
#8438=CYLINDRICAL_SURFACE('',#10700,0.0555000000000001);
#8439=CYLINDRICAL_SURFACE('',#10701,1.24783954473516);
#8440=CYLINDRICAL_SURFACE('',#10702,0.0555000000000001);
#8441=CYLINDRICAL_SURFACE('',#10703,1.24783954473516);
#8442=CYLINDRICAL_SURFACE('',#10704,0.0555000000000001);
#8443=CYLINDRICAL_SURFACE('',#10705,1.24783954473516);
#8444=CYLINDRICAL_SURFACE('',#10706,0.0555000000000001);
#8445=CYLINDRICAL_SURFACE('',#10707,1.24783954473516);
#8446=CYLINDRICAL_SURFACE('',#10708,0.0555000000000001);
#8447=CYLINDRICAL_SURFACE('',#10709,1.24783954473516);
#8448=CYLINDRICAL_SURFACE('',#10710,0.0555000000000001);
#8449=CYLINDRICAL_SURFACE('',#10711,1.24783954473516);
#8450=CYLINDRICAL_SURFACE('',#10712,0.0555000000000001);
#8451=CYLINDRICAL_SURFACE('',#10713,1.24783954473516);
#8452=CYLINDRICAL_SURFACE('',#10714,0.0555000000000001);
#8453=CYLINDRICAL_SURFACE('',#10715,1.24783954473516);
#8454=CYLINDRICAL_SURFACE('',#10716,0.0555000000000001);
#8455=CYLINDRICAL_SURFACE('',#10717,1.24783954473516);
#8456=CYLINDRICAL_SURFACE('',#10718,0.0555000000000001);
#8457=CYLINDRICAL_SURFACE('',#10719,1.24783954473516);
#8458=CYLINDRICAL_SURFACE('',#10725,0.35);
#8459=CYLINDRICAL_SURFACE('',#10733,0.1954);
#8460=ADVANCED_FACE('',(#962),#8181,.F.);
#8461=ADVANCED_FACE('',(#963),#8182,.F.);
#8462=ADVANCED_FACE('',(#964,#637,#638,#639,#640),#773,.F.);
#8463=ADVANCED_FACE('',(#965),#774,.F.);
#8464=ADVANCED_FACE('',(#966),#775,.F.);
#8465=ADVANCED_FACE('',(#967),#8183,.F.);
#8466=ADVANCED_FACE('',(#968),#8184,.F.);
#8467=ADVANCED_FACE('',(#969),#776,.F.);
#8468=ADVANCED_FACE('',(#970),#777,.F.);
#8469=ADVANCED_FACE('',(#971),#8185,.F.);
#8470=ADVANCED_FACE('',(#972),#8186,.F.);
#8471=ADVANCED_FACE('',(#973),#778,.F.);
#8472=ADVANCED_FACE('',(#974),#779,.F.);
#8473=ADVANCED_FACE('',(#975),#8187,.F.);
#8474=ADVANCED_FACE('',(#976),#8188,.F.);
#8475=ADVANCED_FACE('',(#977),#780,.F.);
#8476=ADVANCED_FACE('',(#978),#781,.F.);
#8477=ADVANCED_FACE('',(#979),#8189,.F.);
#8478=ADVANCED_FACE('',(#980),#782,.T.);
#8479=ADVANCED_FACE('',(#981),#8190,.F.);
#8480=ADVANCED_FACE('',(#982),#783,.T.);
#8481=ADVANCED_FACE('',(#983),#8191,.F.);
#8482=ADVANCED_FACE('',(#984),#784,.T.);
#8483=ADVANCED_FACE('',(#985),#8192,.F.);
#8484=ADVANCED_FACE('',(#986),#785,.T.);
#8485=ADVANCED_FACE('',(#987),#786,.T.);
#8486=ADVANCED_FACE('',(#988),#787,.T.);
#8487=ADVANCED_FACE('',(#989),#788,.T.);
#8488=ADVANCED_FACE('',(#990),#789,.T.);
#8489=ADVANCED_FACE('',(#991,#641,#642,#643,#644,#645,#646),#790,.T.);
#8490=ADVANCED_FACE('',(#992),#791,.T.);
#8491=ADVANCED_FACE('',(#993),#792,.T.);
#8492=ADVANCED_FACE('',(#994),#793,.T.);
#8493=ADVANCED_FACE('',(#995),#794,.T.);
#8494=ADVANCED_FACE('',(#996),#795,.T.);
#8495=ADVANCED_FACE('',(#997),#796,.F.);
#8496=ADVANCED_FACE('',(#998),#797,.T.);
#8497=ADVANCED_FACE('',(#999),#798,.T.);
#8498=ADVANCED_FACE('',(#1000),#799,.T.);
#8499=ADVANCED_FACE('',(#1001),#800,.T.);
#8500=ADVANCED_FACE('',(#1002),#801,.T.);
#8501=ADVANCED_FACE('',(#1003),#802,.F.);
#8502=ADVANCED_FACE('',(#1004),#8193,.F.);
#8503=ADVANCED_FACE('',(#1005),#8194,.F.);
#8504=ADVANCED_FACE('',(#1006),#8195,.F.);
#8505=ADVANCED_FACE('',(#1007),#8196,.F.);
#8506=ADVANCED_FACE('',(#1008),#8197,.F.);
#8507=ADVANCED_FACE('',(#1009),#8198,.F.);
#8508=ADVANCED_FACE('',(#1010),#8199,.F.);
#8509=ADVANCED_FACE('',(#1011),#8200,.F.);
#8510=ADVANCED_FACE('',(#1012),#8201,.F.);
#8511=ADVANCED_FACE('',(#1013,#647,#648),#803,.T.);
#8512=ADVANCED_FACE('',(#1014,#649,#650),#804,.T.);
#8513=ADVANCED_FACE('',(#1015),#805,.T.);
#8514=ADVANCED_FACE('',(#1016),#806,.T.);
#8515=ADVANCED_FACE('',(#1017,#651,#652,#653,#654,#655),#807,.T.);
#8516=ADVANCED_FACE('',(#1018),#808,.T.);
#8517=ADVANCED_FACE('',(#1019,#656,#657,#658,#659,#660),#809,.T.);
#8518=ADVANCED_FACE('',(#1020),#810,.T.);
#8519=ADVANCED_FACE('',(#1021),#811,.T.);
#8520=ADVANCED_FACE('',(#1022,#661,#662,#663,#664),#812,.F.);
#8521=ADVANCED_FACE('',(#1023),#8202,.F.);
#8522=ADVANCED_FACE('',(#1024),#8203,.T.);
#8523=ADVANCED_FACE('',(#1025,#665),#813,.T.);
#8524=ADVANCED_FACE('',(#1026,#666),#814,.F.);
#8525=ADVANCED_FACE('',(#1027),#8204,.F.);
#8526=ADVANCED_FACE('',(#1028),#8205,.F.);
#8527=ADVANCED_FACE('',(#1029),#8206,.F.);
#8528=ADVANCED_FACE('',(#1030),#8207,.F.);
#8529=ADVANCED_FACE('',(#1031,#667),#815,.F.);
#8530=ADVANCED_FACE('',(#1032),#8208,.T.);
#8531=ADVANCED_FACE('',(#1033),#8209,.T.);
#8532=ADVANCED_FACE('',(#1034),#8210,.T.);
#8533=ADVANCED_FACE('',(#1035),#8211,.T.);
#8534=ADVANCED_FACE('',(#1036),#8212,.T.);
#8535=ADVANCED_FACE('',(#1037,#668),#816,.T.);
#8536=ADVANCED_FACE('',(#1038),#8213,.F.);
#8537=ADVANCED_FACE('',(#1039,#669),#817,.T.);
#8538=ADVANCED_FACE('',(#1040),#8214,.F.);
#8539=ADVANCED_FACE('',(#1041),#8215,.F.);
#8540=ADVANCED_FACE('',(#1042),#8216,.F.);
#8541=ADVANCED_FACE('',(#1043),#8217,.F.);
#8542=ADVANCED_FACE('',(#1044,#670),#818,.F.);
#8543=ADVANCED_FACE('',(#1045),#8218,.T.);
#8544=ADVANCED_FACE('',(#1046),#8219,.T.);
#8545=ADVANCED_FACE('',(#1047),#8220,.T.);
#8546=ADVANCED_FACE('',(#1048),#8221,.T.);
#8547=ADVANCED_FACE('',(#1049),#8222,.T.);
#8548=ADVANCED_FACE('',(#1050,#671),#819,.F.);
#8549=ADVANCED_FACE('',(#1051),#8223,.F.);
#8550=ADVANCED_FACE('',(#1052,#672),#820,.T.);
#8551=ADVANCED_FACE('',(#1053),#8224,.F.);
#8552=ADVANCED_FACE('',(#1054),#8225,.F.);
#8553=ADVANCED_FACE('',(#1055),#8226,.F.);
#8554=ADVANCED_FACE('',(#1056),#8227,.F.);
#8555=ADVANCED_FACE('',(#1057),#8228,.F.);
#8556=ADVANCED_FACE('',(#1058),#8229,.F.);
#8557=ADVANCED_FACE('',(#1059),#8230,.F.);
#8558=ADVANCED_FACE('',(#1060),#8231,.F.);
#8559=ADVANCED_FACE('',(#1061),#8232,.F.);
#8560=ADVANCED_FACE('',(#1062,#673,#674),#821,.T.);
#8561=ADVANCED_FACE('',(#1063,#675,#676),#822,.T.);
#8562=ADVANCED_FACE('',(#1064),#823,.T.);
#8563=ADVANCED_FACE('',(#1065),#824,.T.);
#8564=ADVANCED_FACE('',(#1066,#677,#678,#679,#680,#681),#825,.T.);
#8565=ADVANCED_FACE('',(#1067),#826,.T.);
#8566=ADVANCED_FACE('',(#1068,#682,#683,#684,#685,#686),#827,.T.);
#8567=ADVANCED_FACE('',(#1069),#828,.T.);
#8568=ADVANCED_FACE('',(#1070),#829,.T.);
#8569=ADVANCED_FACE('',(#1071,#687,#688,#689,#690),#830,.F.);
#8570=ADVANCED_FACE('',(#1072),#8233,.F.);
#8571=ADVANCED_FACE('',(#1073),#8234,.T.);
#8572=ADVANCED_FACE('',(#1074,#691),#831,.T.);
#8573=ADVANCED_FACE('',(#1075,#692),#832,.F.);
#8574=ADVANCED_FACE('',(#1076),#8235,.F.);
#8575=ADVANCED_FACE('',(#1077),#8236,.T.);
#8576=ADVANCED_FACE('',(#1078,#693),#833,.T.);
#8577=ADVANCED_FACE('',(#1079,#694),#834,.F.);
#8578=ADVANCED_FACE('',(#1080),#8237,.F.);
#8579=ADVANCED_FACE('',(#1081),#8238,.T.);
#8580=ADVANCED_FACE('',(#1082,#695),#835,.T.);
#8581=ADVANCED_FACE('',(#1083,#696),#836,.F.);
#8582=ADVANCED_FACE('',(#1084),#8239,.F.);
#8583=ADVANCED_FACE('',(#1085),#8240,.T.);
#8584=ADVANCED_FACE('',(#1086,#697),#837,.T.);
#8585=ADVANCED_FACE('',(#1087,#698),#838,.F.);
#8586=ADVANCED_FACE('',(#1088),#8241,.F.);
#8587=ADVANCED_FACE('',(#1089),#8242,.T.);
#8588=ADVANCED_FACE('',(#1090,#699),#839,.T.);
#8589=ADVANCED_FACE('',(#1091,#700),#840,.F.);
#8590=ADVANCED_FACE('',(#1092),#8243,.F.);
#8591=ADVANCED_FACE('',(#1093),#8244,.F.);
#8592=ADVANCED_FACE('',(#1094),#8245,.F.);
#8593=ADVANCED_FACE('',(#1095),#8246,.F.);
#8594=ADVANCED_FACE('',(#1096,#701),#841,.F.);
#8595=ADVANCED_FACE('',(#1097),#8247,.T.);
#8596=ADVANCED_FACE('',(#1098),#8248,.T.);
#8597=ADVANCED_FACE('',(#1099),#8249,.T.);
#8598=ADVANCED_FACE('',(#1100),#8250,.T.);
#8599=ADVANCED_FACE('',(#1101),#8251,.T.);
#8600=ADVANCED_FACE('',(#1102,#702),#842,.T.);
#8601=ADVANCED_FACE('',(#1103),#8252,.F.);
#8602=ADVANCED_FACE('',(#1104,#703),#843,.T.);
#8603=ADVANCED_FACE('',(#1105),#8253,.F.);
#8604=ADVANCED_FACE('',(#1106),#8254,.F.);
#8605=ADVANCED_FACE('',(#1107),#8255,.F.);
#8606=ADVANCED_FACE('',(#1108),#8256,.F.);
#8607=ADVANCED_FACE('',(#1109,#704),#844,.F.);
#8608=ADVANCED_FACE('',(#1110),#8257,.T.);
#8609=ADVANCED_FACE('',(#1111),#8258,.T.);
#8610=ADVANCED_FACE('',(#1112),#8259,.T.);
#8611=ADVANCED_FACE('',(#1113),#8260,.T.);
#8612=ADVANCED_FACE('',(#1114),#8261,.T.);
#8613=ADVANCED_FACE('',(#1115,#705),#845,.F.);
#8614=ADVANCED_FACE('',(#1116),#8262,.F.);
#8615=ADVANCED_FACE('',(#1117,#706),#846,.T.);
#8616=ADVANCED_FACE('',(#1118),#847,.F.);
#8617=ADVANCED_FACE('',(#1119),#848,.F.);
#8618=ADVANCED_FACE('',(#1120,#707),#849,.F.);
#8619=ADVANCED_FACE('',(#1121),#8263,.F.);
#8620=ADVANCED_FACE('',(#1122),#8264,.F.);
#8621=ADVANCED_FACE('',(#1123),#8265,.T.);
#8622=ADVANCED_FACE('',(#1124),#850,.T.);
#8623=ADVANCED_FACE('',(#1125),#851,.T.);
#8624=ADVANCED_FACE('',(#1126),#8266,.T.);
#8625=ADVANCED_FACE('',(#1127,#708),#852,.T.);
#8626=ADVANCED_FACE('',(#1128),#434,.F.);
#8627=ADVANCED_FACE('',(#1129),#8267,.T.);
#8628=ADVANCED_FACE('',(#1130),#8268,.F.);
#8629=ADVANCED_FACE('',(#1131),#415,.F.);
#8630=ADVANCED_FACE('',(#1132,#709),#853,.T.);
#8631=ADVANCED_FACE('',(#1133),#8269,.T.);
#8632=ADVANCED_FACE('',(#1134,#710),#854,.T.);
#8633=ADVANCED_FACE('',(#1135),#416,.F.);
#8634=ADVANCED_FACE('',(#1136),#435,.F.);
#8635=ADVANCED_FACE('',(#1137),#8270,.F.);
#8636=ADVANCED_FACE('',(#1138,#711),#855,.T.);
#8637=ADVANCED_FACE('',(#1139),#417,.T.);
#8638=ADVANCED_FACE('',(#1140),#8271,.T.);
#8639=ADVANCED_FACE('',(#1141),#418,.T.);
#8640=ADVANCED_FACE('',(#1142,#712),#856,.T.);
#8641=ADVANCED_FACE('',(#1143),#8272,.F.);
#8642=ADVANCED_FACE('',(#1144),#385,.T.);
#8643=ADVANCED_FACE('',(#1145),#386,.T.);
#8644=ADVANCED_FACE('',(#1146),#387,.T.);
#8645=ADVANCED_FACE('',(#1147),#388,.T.);
#8646=ADVANCED_FACE('',(#1148),#389,.T.);
#8647=ADVANCED_FACE('',(#1149),#390,.T.);
#8648=ADVANCED_FACE('',(#1150),#391,.T.);
#8649=ADVANCED_FACE('',(#1151),#392,.T.);
#8650=ADVANCED_FACE('',(#1152),#393,.F.);
#8651=ADVANCED_FACE('',(#1153),#8273,.T.);
#8652=ADVANCED_FACE('',(#1154),#857,.T.);
#8653=ADVANCED_FACE('',(#1155),#394,.F.);
#8654=ADVANCED_FACE('',(#1156),#858,.T.);
#8655=ADVANCED_FACE('',(#1157),#395,.F.);
#8656=ADVANCED_FACE('',(#1158),#859,.T.);
#8657=ADVANCED_FACE('',(#1159),#396,.F.);
#8658=ADVANCED_FACE('',(#1160),#860,.T.);
#8659=ADVANCED_FACE('',(#1161),#397,.F.);
#8660=ADVANCED_FACE('',(#1162),#861,.T.);
#8661=ADVANCED_FACE('',(#1163),#398,.F.);
#8662=ADVANCED_FACE('',(#1164),#862,.T.);
#8663=ADVANCED_FACE('',(#1165),#399,.F.);
#8664=ADVANCED_FACE('',(#1166),#8274,.F.);
#8665=ADVANCED_FACE('',(#1167),#863,.T.);
#8666=ADVANCED_FACE('',(#1168),#400,.F.);
#8667=ADVANCED_FACE('',(#1169,#713),#864,.T.);
#8668=ADVANCED_FACE('',(#1170),#865,.T.);
#8669=ADVANCED_FACE('',(#1171,#714),#866,.T.);
#8670=ADVANCED_FACE('',(#1172),#8275,.T.);
#8671=ADVANCED_FACE('',(#1173,#715),#867,.T.);
#8672=ADVANCED_FACE('',(#1174),#8276,.F.);
#8673=ADVANCED_FACE('',(#1175,#716),#868,.T.);
#8674=ADVANCED_FACE('',(#1176),#8277,.T.);
#8675=ADVANCED_FACE('',(#1177,#717),#869,.T.);
#8676=ADVANCED_FACE('',(#1178),#8278,.F.);
#8677=ADVANCED_FACE('',(#1179),#870,.F.);
#8678=ADVANCED_FACE('',(#1180),#871,.F.);
#8679=ADVANCED_FACE('',(#1181),#872,.F.);
#8680=ADVANCED_FACE('',(#1182),#873,.F.);
#8681=ADVANCED_FACE('',(#1183),#874,.F.);
#8682=ADVANCED_FACE('',(#1184),#875,.F.);
#8683=ADVANCED_FACE('',(#1185),#876,.F.);
#8684=ADVANCED_FACE('',(#1186),#877,.F.);
#8685=ADVANCED_FACE('',(#1187,#718),#878,.T.);
#8686=ADVANCED_FACE('',(#1188),#8279,.T.);
#8687=ADVANCED_FACE('',(#1189),#879,.F.);
#8688=ADVANCED_FACE('',(#1190),#880,.T.);
#8689=ADVANCED_FACE('',(#1191),#419,.T.);
#8690=ADVANCED_FACE('',(#1192),#8280,.T.);
#8691=ADVANCED_FACE('',(#1193),#420,.T.);
#8692=ADVANCED_FACE('',(#1194,#719),#881,.T.);
#8693=ADVANCED_FACE('',(#1195),#421,.T.);
#8694=ADVANCED_FACE('',(#1196),#8281,.T.);
#8695=ADVANCED_FACE('',(#1197),#422,.T.);
#8696=ADVANCED_FACE('',(#1198),#436,.F.);
#8697=ADVANCED_FACE('',(#1199),#8282,.T.);
#8698=ADVANCED_FACE('',(#1200),#8283,.F.);
#8699=ADVANCED_FACE('',(#1201),#423,.F.);
#8700=ADVANCED_FACE('',(#1202,#720),#882,.T.);
#8701=ADVANCED_FACE('',(#1203),#8284,.T.);
#8702=ADVANCED_FACE('',(#1204,#721),#883,.T.);
#8703=ADVANCED_FACE('',(#1205),#424,.F.);
#8704=ADVANCED_FACE('',(#1206),#437,.F.);
#8705=ADVANCED_FACE('',(#1207),#8285,.F.);
#8706=ADVANCED_FACE('',(#1208,#722),#884,.T.);
#8707=ADVANCED_FACE('',(#1209),#425,.T.);
#8708=ADVANCED_FACE('',(#1210),#8286,.T.);
#8709=ADVANCED_FACE('',(#1211),#426,.T.);
#8710=ADVANCED_FACE('',(#1212,#723),#885,.T.);
#8711=ADVANCED_FACE('',(#1213),#8287,.F.);
#8712=ADVANCED_FACE('',(#1214),#401,.T.);
#8713=ADVANCED_FACE('',(#1215),#402,.T.);
#8714=ADVANCED_FACE('',(#1216),#403,.T.);
#8715=ADVANCED_FACE('',(#1217),#404,.T.);
#8716=ADVANCED_FACE('',(#1218),#405,.T.);
#8717=ADVANCED_FACE('',(#1219),#406,.T.);
#8718=ADVANCED_FACE('',(#1220),#407,.T.);
#8719=ADVANCED_FACE('',(#1221),#408,.F.);
#8720=ADVANCED_FACE('',(#1222),#8288,.T.);
#8721=ADVANCED_FACE('',(#1223),#886,.T.);
#8722=ADVANCED_FACE('',(#1224),#409,.F.);
#8723=ADVANCED_FACE('',(#1225),#887,.T.);
#8724=ADVANCED_FACE('',(#1226),#410,.F.);
#8725=ADVANCED_FACE('',(#1227),#888,.T.);
#8726=ADVANCED_FACE('',(#1228),#411,.F.);
#8727=ADVANCED_FACE('',(#1229),#889,.T.);
#8728=ADVANCED_FACE('',(#1230),#412,.F.);
#8729=ADVANCED_FACE('',(#1231),#890,.T.);
#8730=ADVANCED_FACE('',(#1232),#413,.F.);
#8731=ADVANCED_FACE('',(#1233),#8289,.F.);
#8732=ADVANCED_FACE('',(#1234),#891,.T.);
#8733=ADVANCED_FACE('',(#1235),#414,.F.);
#8734=ADVANCED_FACE('',(#1236,#724),#892,.T.);
#8735=ADVANCED_FACE('',(#1237),#893,.T.);
#8736=ADVANCED_FACE('',(#1238,#725),#894,.T.);
#8737=ADVANCED_FACE('',(#1239),#8290,.T.);
#8738=ADVANCED_FACE('',(#1240,#726),#895,.T.);
#8739=ADVANCED_FACE('',(#1241),#8291,.F.);
#8740=ADVANCED_FACE('',(#1242,#727),#896,.T.);
#8741=ADVANCED_FACE('',(#1243),#8292,.T.);
#8742=ADVANCED_FACE('',(#1244,#728),#897,.T.);
#8743=ADVANCED_FACE('',(#1245),#8293,.F.);
#8744=ADVANCED_FACE('',(#1246),#898,.F.);
#8745=ADVANCED_FACE('',(#1247),#899,.F.);
#8746=ADVANCED_FACE('',(#1248),#900,.F.);
#8747=ADVANCED_FACE('',(#1249),#901,.F.);
#8748=ADVANCED_FACE('',(#1250),#902,.F.);
#8749=ADVANCED_FACE('',(#1251),#903,.F.);
#8750=ADVANCED_FACE('',(#1252),#904,.F.);
#8751=ADVANCED_FACE('',(#1253),#905,.F.);
#8752=ADVANCED_FACE('',(#1254),#906,.F.);
#8753=ADVANCED_FACE('',(#1255),#907,.T.);
#8754=ADVANCED_FACE('',(#1256),#427,.T.);
#8755=ADVANCED_FACE('',(#1257),#8294,.T.);
#8756=ADVANCED_FACE('',(#1258),#428,.T.);
#8757=ADVANCED_FACE('',(#1259,#729),#908,.T.);
#8758=ADVANCED_FACE('',(#1260),#429,.T.);
#8759=ADVANCED_FACE('',(#1261),#8295,.T.);
#8760=ADVANCED_FACE('',(#1262),#8296,.F.);
#8761=ADVANCED_FACE('',(#1263),#909,.F.);
#8762=ADVANCED_FACE('',(#1264,#730),#910,.T.);
#8763=ADVANCED_FACE('',(#1265,#731),#911,.F.);
#8764=ADVANCED_FACE('',(#1266),#8297,.T.);
#8765=ADVANCED_FACE('',(#1267),#8298,.T.);
#8766=ADVANCED_FACE('',(#1268),#8299,.T.);
#8767=ADVANCED_FACE('',(#1269,#732),#912,.F.);
#8768=ADVANCED_FACE('',(#1270),#8300,.T.);
#8769=ADVANCED_FACE('',(#1271),#913,.T.);
#8770=ADVANCED_FACE('',(#1272,#733),#914,.F.);
#8771=ADVANCED_FACE('',(#1273),#8301,.F.);
#8772=ADVANCED_FACE('',(#1274,#734),#915,.T.);
#8773=ADVANCED_FACE('',(#1275),#8302,.F.);
#8774=ADVANCED_FACE('',(#1276),#8303,.T.);
#8775=ADVANCED_FACE('',(#1277,#735),#916,.T.);
#8776=ADVANCED_FACE('',(#1278,#736),#917,.F.);
#8777=ADVANCED_FACE('',(#1279),#8304,.F.);
#8778=ADVANCED_FACE('',(#1280),#8305,.T.);
#8779=ADVANCED_FACE('',(#1281,#737),#918,.T.);
#8780=ADVANCED_FACE('',(#1282,#738),#919,.F.);
#8781=ADVANCED_FACE('',(#1283),#8306,.T.);
#8782=ADVANCED_FACE('',(#1284),#920,.T.);
#8783=ADVANCED_FACE('',(#1285),#921,.F.);
#8784=ADVANCED_FACE('',(#1286),#8307,.T.);
#8785=ADVANCED_FACE('',(#1287),#922,.T.);
#8786=ADVANCED_FACE('',(#1288),#923,.F.);
#8787=ADVANCED_FACE('',(#1289),#8308,.F.);
#8788=ADVANCED_FACE('',(#1290),#8309,.T.);
#8789=ADVANCED_FACE('',(#1291,#739),#924,.T.);
#8790=ADVANCED_FACE('',(#1292,#740),#925,.F.);
#8791=ADVANCED_FACE('',(#1293),#8310,.F.);
#8792=ADVANCED_FACE('',(#1294),#8311,.F.);
#8793=ADVANCED_FACE('',(#1295,#741,#742,#743),#8312,.T.);
#8794=ADVANCED_FACE('',(#1296),#8313,.F.);
#8795=ADVANCED_FACE('',(#1297),#8314,.F.);
#8796=ADVANCED_FACE('',(#1298,#744,#745,#746),#8315,.F.);
#8797=ADVANCED_FACE('',(#1299,#747),#926,.F.);
#8798=ADVANCED_FACE('',(#1300,#748),#927,.T.);
#8799=ADVANCED_FACE('',(#1301),#8316,.T.);
#8800=ADVANCED_FACE('',(#1302,#749),#928,.F.);
#8801=ADVANCED_FACE('',(#1303,#750),#929,.F.);
#8802=ADVANCED_FACE('',(#1304),#8317,.T.);
#8803=ADVANCED_FACE('',(#1305,#751),#930,.T.);
#8804=ADVANCED_FACE('',(#1306),#8318,.F.);
#8805=ADVANCED_FACE('',(#1307),#8319,.T.);
#8806=ADVANCED_FACE('',(#1308),#8320,.F.);
#8807=ADVANCED_FACE('',(#1309),#8321,.T.);
#8808=ADVANCED_FACE('',(#1310),#8322,.F.);
#8809=ADVANCED_FACE('',(#1311),#8323,.T.);
#8810=ADVANCED_FACE('',(#1312),#8324,.F.);
#8811=ADVANCED_FACE('',(#1313),#8325,.T.);
#8812=ADVANCED_FACE('',(#1314),#8326,.F.);
#8813=ADVANCED_FACE('',(#1315),#8327,.T.);
#8814=ADVANCED_FACE('',(#1316),#8328,.F.);
#8815=ADVANCED_FACE('',(#1317),#8329,.T.);
#8816=ADVANCED_FACE('',(#1318),#8330,.F.);
#8817=ADVANCED_FACE('',(#1319),#8331,.T.);
#8818=ADVANCED_FACE('',(#1320),#8332,.F.);
#8819=ADVANCED_FACE('',(#1321),#8333,.T.);
#8820=ADVANCED_FACE('',(#1322),#8334,.F.);
#8821=ADVANCED_FACE('',(#1323),#8335,.T.);
#8822=ADVANCED_FACE('',(#1324),#8336,.F.);
#8823=ADVANCED_FACE('',(#1325),#8337,.T.);
#8824=ADVANCED_FACE('',(#1326),#8338,.F.);
#8825=ADVANCED_FACE('',(#1327),#8339,.T.);
#8826=ADVANCED_FACE('',(#1328),#8340,.F.);
#8827=ADVANCED_FACE('',(#1329),#8341,.T.);
#8828=ADVANCED_FACE('',(#1330),#8342,.F.);
#8829=ADVANCED_FACE('',(#1331),#8343,.T.);
#8830=ADVANCED_FACE('',(#1332),#8344,.F.);
#8831=ADVANCED_FACE('',(#1333),#8345,.T.);
#8832=ADVANCED_FACE('',(#1334),#8346,.F.);
#8833=ADVANCED_FACE('',(#1335),#8347,.T.);
#8834=ADVANCED_FACE('',(#1336),#8348,.F.);
#8835=ADVANCED_FACE('',(#1337),#8349,.T.);
#8836=ADVANCED_FACE('',(#1338),#8350,.F.);
#8837=ADVANCED_FACE('',(#1339),#8351,.T.);
#8838=ADVANCED_FACE('',(#1340),#8352,.F.);
#8839=ADVANCED_FACE('',(#1341),#8353,.T.);
#8840=ADVANCED_FACE('',(#1342),#8354,.F.);
#8841=ADVANCED_FACE('',(#1343),#8355,.T.);
#8842=ADVANCED_FACE('',(#1344),#8356,.F.);
#8843=ADVANCED_FACE('',(#1345),#8357,.T.);
#8844=ADVANCED_FACE('',(#1346),#8358,.F.);
#8845=ADVANCED_FACE('',(#1347),#931,.F.);
#8846=ADVANCED_FACE('',(#1348,#752),#932,.T.);
#8847=ADVANCED_FACE('',(#1349,#753),#933,.F.);
#8848=ADVANCED_FACE('',(#1350),#8359,.T.);
#8849=ADVANCED_FACE('',(#1351),#8360,.T.);
#8850=ADVANCED_FACE('',(#1352,#754),#934,.F.);
#8851=ADVANCED_FACE('',(#1353),#8361,.T.);
#8852=ADVANCED_FACE('',(#1354),#935,.T.);
#8853=ADVANCED_FACE('',(#1355),#8362,.F.);
#8854=ADVANCED_FACE('',(#1356),#8363,.T.);
#8855=ADVANCED_FACE('',(#1357,#755),#936,.T.);
#8856=ADVANCED_FACE('',(#1358,#756),#937,.F.);
#8857=ADVANCED_FACE('',(#1359),#8364,.F.);
#8858=ADVANCED_FACE('',(#1360),#8365,.T.);
#8859=ADVANCED_FACE('',(#1361,#757),#938,.T.);
#8860=ADVANCED_FACE('',(#1362,#758),#939,.F.);
#8861=ADVANCED_FACE('',(#1363),#8366,.T.);
#8862=ADVANCED_FACE('',(#1364),#940,.T.);
#8863=ADVANCED_FACE('',(#1365),#941,.F.);
#8864=ADVANCED_FACE('',(#1366),#8367,.T.);
#8865=ADVANCED_FACE('',(#1367),#942,.T.);
#8866=ADVANCED_FACE('',(#1368),#943,.F.);
#8867=ADVANCED_FACE('',(#1369),#8368,.F.);
#8868=ADVANCED_FACE('',(#1370),#8369,.T.);
#8869=ADVANCED_FACE('',(#1371,#759),#944,.T.);
#8870=ADVANCED_FACE('',(#1372,#760),#945,.F.);
#8871=ADVANCED_FACE('',(#1373),#8370,.F.);
#8872=ADVANCED_FACE('',(#1374),#8371,.F.);
#8873=ADVANCED_FACE('',(#1375,#761,#762,#763),#8372,.T.);
#8874=ADVANCED_FACE('',(#1376),#8373,.F.);
#8875=ADVANCED_FACE('',(#1377),#8374,.F.);
#8876=ADVANCED_FACE('',(#1378,#764,#765,#766),#8375,.F.);
#8877=ADVANCED_FACE('',(#1379,#767),#946,.F.);
#8878=ADVANCED_FACE('',(#1380,#768),#947,.T.);
#8879=ADVANCED_FACE('',(#1381),#8376,.T.);
#8880=ADVANCED_FACE('',(#1382,#769),#948,.F.);
#8881=ADVANCED_FACE('',(#1383,#770),#949,.F.);
#8882=ADVANCED_FACE('',(#1384),#8377,.T.);
#8883=ADVANCED_FACE('',(#1385,#771),#950,.T.);
#8884=ADVANCED_FACE('',(#1386),#8378,.F.);
#8885=ADVANCED_FACE('',(#1387),#8379,.T.);
#8886=ADVANCED_FACE('',(#1388),#8380,.F.);
#8887=ADVANCED_FACE('',(#1389),#8381,.T.);
#8888=ADVANCED_FACE('',(#1390),#8382,.F.);
#8889=ADVANCED_FACE('',(#1391),#8383,.T.);
#8890=ADVANCED_FACE('',(#1392),#8384,.F.);
#8891=ADVANCED_FACE('',(#1393),#8385,.T.);
#8892=ADVANCED_FACE('',(#1394),#8386,.F.);
#8893=ADVANCED_FACE('',(#1395),#8387,.T.);
#8894=ADVANCED_FACE('',(#1396),#8388,.F.);
#8895=ADVANCED_FACE('',(#1397),#8389,.T.);
#8896=ADVANCED_FACE('',(#1398),#8390,.F.);
#8897=ADVANCED_FACE('',(#1399),#8391,.T.);
#8898=ADVANCED_FACE('',(#1400),#8392,.F.);
#8899=ADVANCED_FACE('',(#1401),#8393,.T.);
#8900=ADVANCED_FACE('',(#1402),#8394,.F.);
#8901=ADVANCED_FACE('',(#1403),#8395,.T.);
#8902=ADVANCED_FACE('',(#1404),#8396,.F.);
#8903=ADVANCED_FACE('',(#1405),#8397,.T.);
#8904=ADVANCED_FACE('',(#1406),#8398,.F.);
#8905=ADVANCED_FACE('',(#1407),#8399,.T.);
#8906=ADVANCED_FACE('',(#1408),#8400,.F.);
#8907=ADVANCED_FACE('',(#1409),#8401,.T.);
#8908=ADVANCED_FACE('',(#1410),#8402,.F.);
#8909=ADVANCED_FACE('',(#1411),#8403,.T.);
#8910=ADVANCED_FACE('',(#1412),#8404,.F.);
#8911=ADVANCED_FACE('',(#1413),#8405,.T.);
#8912=ADVANCED_FACE('',(#1414),#8406,.F.);
#8913=ADVANCED_FACE('',(#1415),#8407,.T.);
#8914=ADVANCED_FACE('',(#1416),#8408,.F.);
#8915=ADVANCED_FACE('',(#1417),#8409,.T.);
#8916=ADVANCED_FACE('',(#1418),#8410,.F.);
#8917=ADVANCED_FACE('',(#1419),#8411,.T.);
#8918=ADVANCED_FACE('',(#1420),#8412,.F.);
#8919=ADVANCED_FACE('',(#1421),#8413,.T.);
#8920=ADVANCED_FACE('',(#1422),#8414,.F.);
#8921=ADVANCED_FACE('',(#1423),#8415,.T.);
#8922=ADVANCED_FACE('',(#1424),#8416,.F.);
#8923=ADVANCED_FACE('',(#1425),#8417,.T.);
#8924=ADVANCED_FACE('',(#1426),#8418,.F.);
#8925=ADVANCED_FACE('',(#1427),#8419,.T.);
#8926=ADVANCED_FACE('',(#1428),#8420,.F.);
#8927=ADVANCED_FACE('',(#1429),#8421,.T.);
#8928=ADVANCED_FACE('',(#1430),#8422,.F.);
#8929=ADVANCED_FACE('',(#1431),#8423,.T.);
#8930=ADVANCED_FACE('',(#1432),#8424,.F.);
#8931=ADVANCED_FACE('',(#1433),#8425,.T.);
#8932=ADVANCED_FACE('',(#1434),#8426,.F.);
#8933=ADVANCED_FACE('',(#1435),#8427,.T.);
#8934=ADVANCED_FACE('',(#1436),#8428,.F.);
#8935=ADVANCED_FACE('',(#1437),#8429,.T.);
#8936=ADVANCED_FACE('',(#1438),#8430,.F.);
#8937=ADVANCED_FACE('',(#1439),#8431,.T.);
#8938=ADVANCED_FACE('',(#1440),#8432,.F.);
#8939=ADVANCED_FACE('',(#1441),#8433,.T.);
#8940=ADVANCED_FACE('',(#1442),#8434,.F.);
#8941=ADVANCED_FACE('',(#1443),#8435,.T.);
#8942=ADVANCED_FACE('',(#1444),#8436,.F.);
#8943=ADVANCED_FACE('',(#1445),#8437,.T.);
#8944=ADVANCED_FACE('',(#1446),#8438,.F.);
#8945=ADVANCED_FACE('',(#1447),#8439,.T.);
#8946=ADVANCED_FACE('',(#1448),#8440,.F.);
#8947=ADVANCED_FACE('',(#1449),#8441,.T.);
#8948=ADVANCED_FACE('',(#1450),#8442,.F.);
#8949=ADVANCED_FACE('',(#1451),#8443,.T.);
#8950=ADVANCED_FACE('',(#1452),#8444,.F.);
#8951=ADVANCED_FACE('',(#1453),#8445,.T.);
#8952=ADVANCED_FACE('',(#1454),#8446,.F.);
#8953=ADVANCED_FACE('',(#1455),#8447,.T.);
#8954=ADVANCED_FACE('',(#1456),#8448,.F.);
#8955=ADVANCED_FACE('',(#1457),#8449,.T.);
#8956=ADVANCED_FACE('',(#1458),#8450,.F.);
#8957=ADVANCED_FACE('',(#1459),#8451,.T.);
#8958=ADVANCED_FACE('',(#1460),#8452,.F.);
#8959=ADVANCED_FACE('',(#1461),#8453,.T.);
#8960=ADVANCED_FACE('',(#1462),#8454,.F.);
#8961=ADVANCED_FACE('',(#1463),#8455,.T.);
#8962=ADVANCED_FACE('',(#1464),#8456,.F.);
#8963=ADVANCED_FACE('',(#1465),#8457,.T.);
#8964=ADVANCED_FACE('',(#1466),#951,.T.);
#8965=ADVANCED_FACE('',(#1467),#430,.T.);
#8966=ADVANCED_FACE('',(#1468),#8458,.T.);
#8967=ADVANCED_FACE('',(#1469),#431,.T.);
#8968=ADVANCED_FACE('',(#1470,#772),#952,.T.);
#8969=ADVANCED_FACE('',(#1471),#432,.T.);
#8970=ADVANCED_FACE('',(#1472),#8459,.T.);
#8971=ADVANCED_FACE('',(#1473),#433,.T.);
#8972=ADVANCED_FACE('',(#1474),#953,.T.);
#8973=ADVANCED_FACE('',(#1475),#954,.F.);
#8974=ADVANCED_FACE('',(#1476),#955,.F.);
#8975=ADVANCED_FACE('',(#1477),#956,.F.);
#8976=ADVANCED_FACE('',(#1478),#957,.F.);
#8977=ADVANCED_FACE('',(#1479),#958,.F.);
#8978=ADVANCED_FACE('',(#1480),#959,.F.);
#8979=ADVANCED_FACE('',(#1481),#960,.F.);
#8980=ADVANCED_FACE('',(#1482),#961,.F.);
#8981=CLOSED_SHELL('',(#8460,#8461,#8462,#8463,#8464,#8465,#8466,#8467,
#8468,#8469,#8470,#8471,#8472,#8473,#8474,#8475,#8476,#8477,#8478,#8479,
#8480,#8481,#8482,#8483,#8484,#8485,#8486,#8487,#8488,#8489));
#8982=CLOSED_SHELL('',(#8490,#8491,#8492,#8493,#8494,#8495));
#8983=CLOSED_SHELL('',(#8496,#8497,#8498,#8499,#8500,#8501));
#8984=CLOSED_SHELL('',(#8502,#8503,#8504,#8505,#8506,#8507,#8508,#8509,
#8510,#8511,#8512,#8513,#8514,#8515,#8516,#8517,#8518,#8519,#8520));
#8985=CLOSED_SHELL('',(#8521,#8522,#8523,#8524));
#8986=CLOSED_SHELL('',(#8525,#8526,#8527,#8528,#8529,#8530,#8531,#8532,
#8533,#8534,#8535,#8536,#8537));
#8987=CLOSED_SHELL('',(#8538,#8539,#8540,#8541,#8542,#8543,#8544,#8545,
#8546,#8547,#8548,#8549,#8550));
#8988=CLOSED_SHELL('',(#8551,#8552,#8553,#8554,#8555,#8556,#8557,#8558,
#8559,#8560,#8561,#8562,#8563,#8564,#8565,#8566,#8567,#8568,#8569));
#8989=CLOSED_SHELL('',(#8570,#8571,#8572,#8573));
#8990=CLOSED_SHELL('',(#8574,#8575,#8576,#8577));
#8991=CLOSED_SHELL('',(#8578,#8579,#8580,#8581));
#8992=CLOSED_SHELL('',(#8582,#8583,#8584,#8585));
#8993=CLOSED_SHELL('',(#8586,#8587,#8588,#8589));
#8994=CLOSED_SHELL('',(#8590,#8591,#8592,#8593,#8594,#8595,#8596,#8597,
#8598,#8599,#8600,#8601,#8602));
#8995=CLOSED_SHELL('',(#8603,#8604,#8605,#8606,#8607,#8608,#8609,#8610,
#8611,#8612,#8613,#8614,#8615));
#8996=CLOSED_SHELL('',(#8616,#8617,#8618,#8619,#8620,#8621,#8622,#8623,
#8624,#8625));
#8997=CLOSED_SHELL('',(#8626,#8627,#8628,#8629,#8630,#8631,#8632,#8633));
#8998=CLOSED_SHELL('',(#8634,#8635,#8636,#8637,#8638,#8639,#8640,#8641));
#8999=CLOSED_SHELL('',(#8642));
#9000=CLOSED_SHELL('',(#8643));
#9001=CLOSED_SHELL('',(#8644));
#9002=CLOSED_SHELL('',(#8645));
#9003=CLOSED_SHELL('',(#8646));
#9004=CLOSED_SHELL('',(#8647));
#9005=CLOSED_SHELL('',(#8648));
#9006=CLOSED_SHELL('',(#8649));
#9007=CLOSED_SHELL('',(#8650,#8651,#8652,#8653,#8654,#8655,#8656,#8657,
#8658,#8659,#8660,#8661,#8662,#8663,#8664,#8665,#8666,#8667,#8668));
#9008=CLOSED_SHELL('',(#8669,#8670,#8671,#8672));
#9009=CLOSED_SHELL('',(#8673,#8674,#8675,#8676));
#9010=CLOSED_SHELL('',(#8677,#8678,#8679,#8680,#8681,#8682,#8683,#8684));
#9011=CLOSED_SHELL('',(#8685,#8686,#8687,#8688,#8689,#8690,#8691,#8692,
#8693,#8694,#8695));
#9012=CLOSED_SHELL('',(#8696,#8697,#8698,#8699,#8700,#8701,#8702,#8703));
#9013=CLOSED_SHELL('',(#8704,#8705,#8706,#8707,#8708,#8709,#8710,#8711));
#9014=CLOSED_SHELL('',(#8712));
#9015=CLOSED_SHELL('',(#8713));
#9016=CLOSED_SHELL('',(#8714));
#9017=CLOSED_SHELL('',(#8715));
#9018=CLOSED_SHELL('',(#8716));
#9019=CLOSED_SHELL('',(#8717));
#9020=CLOSED_SHELL('',(#8718));
#9021=CLOSED_SHELL('',(#8719,#8720,#8721,#8722,#8723,#8724,#8725,#8726,
#8727,#8728,#8729,#8730,#8731,#8732,#8733,#8734,#8735));
#9022=CLOSED_SHELL('',(#8736,#8737,#8738,#8739));
#9023=CLOSED_SHELL('',(#8740,#8741,#8742,#8743));
#9024=CLOSED_SHELL('',(#8744,#8745,#8746,#8747,#8748,#8749,#8750,#8751));
#9025=CLOSED_SHELL('',(#8752,#8753,#8754,#8755,#8756,#8757,#8758,#8759));
#9026=CLOSED_SHELL('',(#8760,#8761,#8762,#8763,#8764,#8765,#8766,#8767,
#8768,#8769,#8770));
#9027=CLOSED_SHELL('',(#8771,#8772,#8773,#8774,#8775,#8776));
#9028=CLOSED_SHELL('',(#8777,#8778,#8779,#8780));
#9029=CLOSED_SHELL('',(#8781,#8782,#8783));
#9030=CLOSED_SHELL('',(#8784,#8785,#8786));
#9031=CLOSED_SHELL('',(#8787,#8788,#8789,#8790));
#9032=CLOSED_SHELL('',(#8791,#8792,#8793,#8794,#8795,#8796,#8797,#8798,
#8799,#8800,#8801,#8802,#8803,#8804,#8805,#8806,#8807,#8808,#8809,#8810,
#8811,#8812,#8813,#8814,#8815,#8816,#8817,#8818,#8819,#8820,#8821,#8822,
#8823,#8824,#8825,#8826,#8827,#8828,#8829,#8830,#8831,#8832,#8833,#8834,
#8835,#8836,#8837,#8838,#8839,#8840,#8841,#8842,#8843));
#9033=CLOSED_SHELL('',(#8844,#8845,#8846,#8847,#8848,#8849,#8850,#8851,
#8852));
#9034=CLOSED_SHELL('',(#8853,#8854,#8855,#8856));
#9035=CLOSED_SHELL('',(#8857,#8858,#8859,#8860));
#9036=CLOSED_SHELL('',(#8861,#8862,#8863));
#9037=CLOSED_SHELL('',(#8864,#8865,#8866));
#9038=CLOSED_SHELL('',(#8867,#8868,#8869,#8870));
#9039=CLOSED_SHELL('',(#8871,#8872,#8873,#8874,#8875,#8876,#8877,#8878,
#8879,#8880,#8881,#8882,#8883,#8884,#8885,#8886,#8887,#8888,#8889,#8890,
#8891,#8892,#8893,#8894,#8895,#8896,#8897,#8898,#8899,#8900,#8901,#8902,
#8903,#8904,#8905,#8906,#8907,#8908,#8909,#8910,#8911,#8912,#8913,#8914,
#8915,#8916,#8917,#8918,#8919,#8920,#8921,#8922,#8923,#8924,#8925,#8926,
#8927,#8928,#8929,#8930,#8931,#8932,#8933,#8934,#8935,#8936,#8937,#8938,
#8939,#8940,#8941,#8942,#8943,#8944,#8945,#8946,#8947,#8948,#8949,#8950,
#8951,#8952,#8953,#8954,#8955,#8956,#8957,#8958,#8959,#8960,#8961,#8962,
#8963));
#9040=CLOSED_SHELL('',(#8964,#8965,#8966,#8967,#8968,#8969,#8970,#8971,
#8972));
#9041=CLOSED_SHELL('',(#8973,#8974,#8975,#8976,#8977,#8978,#8979,#8980));
#9042=DERIVED_UNIT_ELEMENT(#9128,1.);
#9043=DERIVED_UNIT_ELEMENT(#17832,-3.);
#9044=DERIVED_UNIT_ELEMENT(#9128,1.);
#9045=DERIVED_UNIT_ELEMENT(#17832,-3.);
#9046=DERIVED_UNIT_ELEMENT(#9128,1.);
#9047=DERIVED_UNIT_ELEMENT(#17832,-3.);
#9048=DERIVED_UNIT_ELEMENT(#9128,1.);
#9049=DERIVED_UNIT_ELEMENT(#17832,-3.);
#9050=DERIVED_UNIT_ELEMENT(#9128,1.);
#9051=DERIVED_UNIT_ELEMENT(#17832,-3.);
#9052=DERIVED_UNIT_ELEMENT(#9128,1.);
#9053=DERIVED_UNIT_ELEMENT(#17832,-3.);
#9054=DERIVED_UNIT_ELEMENT(#9128,1.);
#9055=DERIVED_UNIT_ELEMENT(#17832,-3.);
#9056=DERIVED_UNIT_ELEMENT(#9128,1.);
#9057=DERIVED_UNIT_ELEMENT(#17832,-3.);
#9058=DERIVED_UNIT_ELEMENT(#9128,1.);
#9059=DERIVED_UNIT_ELEMENT(#17832,-3.);
#9060=DERIVED_UNIT_ELEMENT(#9128,1.);
#9061=DERIVED_UNIT_ELEMENT(#17832,-3.);
#9062=DERIVED_UNIT_ELEMENT(#9128,1.);
#9063=DERIVED_UNIT_ELEMENT(#17832,-3.);
#9064=DERIVED_UNIT_ELEMENT(#9128,1.);
#9065=DERIVED_UNIT_ELEMENT(#17832,-3.);
#9066=DERIVED_UNIT_ELEMENT(#9128,1.);
#9067=DERIVED_UNIT_ELEMENT(#17832,-3.);
#9068=DERIVED_UNIT_ELEMENT(#9128,1.);
#9069=DERIVED_UNIT_ELEMENT(#17832,-3.);
#9070=DERIVED_UNIT_ELEMENT(#9128,1.);
#9071=DERIVED_UNIT_ELEMENT(#17832,-3.);
#9072=DERIVED_UNIT_ELEMENT(#9128,1.);
#9073=DERIVED_UNIT_ELEMENT(#17832,-3.);
#9074=DERIVED_UNIT_ELEMENT(#9128,1.);
#9075=DERIVED_UNIT_ELEMENT(#17832,-3.);
#9076=DERIVED_UNIT_ELEMENT(#9128,1.);
#9077=DERIVED_UNIT_ELEMENT(#17832,-3.);
#9078=DERIVED_UNIT_ELEMENT(#9128,1.);
#9079=DERIVED_UNIT_ELEMENT(#17832,-3.);
#9080=DERIVED_UNIT_ELEMENT(#9128,1.);
#9081=DERIVED_UNIT_ELEMENT(#17832,-3.);
#9082=DERIVED_UNIT_ELEMENT(#9128,1.);
#9083=DERIVED_UNIT_ELEMENT(#17832,-3.);
#9084=DERIVED_UNIT_ELEMENT(#9128,1.);
#9085=DERIVED_UNIT_ELEMENT(#17832,-3.);
#9086=DERIVED_UNIT_ELEMENT(#9128,1.);
#9087=DERIVED_UNIT_ELEMENT(#17832,-3.);
#9088=DERIVED_UNIT_ELEMENT(#9128,1.);
#9089=DERIVED_UNIT_ELEMENT(#17832,-3.);
#9090=DERIVED_UNIT_ELEMENT(#9128,1.);
#9091=DERIVED_UNIT_ELEMENT(#17832,-3.);
#9092=DERIVED_UNIT_ELEMENT(#9128,1.);
#9093=DERIVED_UNIT_ELEMENT(#17832,-3.);
#9094=DERIVED_UNIT_ELEMENT(#9128,1.);
#9095=DERIVED_UNIT_ELEMENT(#17832,-3.);
#9096=DERIVED_UNIT_ELEMENT(#9128,1.);
#9097=DERIVED_UNIT_ELEMENT(#17832,-3.);
#9098=DERIVED_UNIT_ELEMENT(#9128,1.);
#9099=DERIVED_UNIT_ELEMENT(#17832,-3.);
#9100=DERIVED_UNIT_ELEMENT(#9128,1.);
#9101=DERIVED_UNIT_ELEMENT(#17832,-3.);
#9102=DERIVED_UNIT_ELEMENT(#9128,1.);
#9103=DERIVED_UNIT_ELEMENT(#17832,-3.);
#9104=DERIVED_UNIT_ELEMENT(#9128,1.);
#9105=DERIVED_UNIT_ELEMENT(#17832,-3.);
#9106=DERIVED_UNIT_ELEMENT(#9128,1.);
#9107=DERIVED_UNIT_ELEMENT(#17832,-3.);
#9108=DERIVED_UNIT_ELEMENT(#9128,1.);
#9109=DERIVED_UNIT_ELEMENT(#17832,-3.);
#9110=DERIVED_UNIT_ELEMENT(#9128,1.);
#9111=DERIVED_UNIT_ELEMENT(#17832,-3.);
#9112=DERIVED_UNIT_ELEMENT(#9128,1.);
#9113=DERIVED_UNIT_ELEMENT(#17832,-3.);
#9114=DERIVED_UNIT_ELEMENT(#9128,1.);
#9115=DERIVED_UNIT_ELEMENT(#17832,-3.);
#9116=DERIVED_UNIT_ELEMENT(#9128,1.);
#9117=DERIVED_UNIT_ELEMENT(#17832,-3.);
#9118=DERIVED_UNIT_ELEMENT(#9128,1.);
#9119=DERIVED_UNIT_ELEMENT(#17832,-3.);
#9120=DERIVED_UNIT_ELEMENT(#9128,1.);
#9121=DERIVED_UNIT_ELEMENT(#17832,-3.);
#9122=DERIVED_UNIT_ELEMENT(#9128,1.);
#9123=DERIVED_UNIT_ELEMENT(#17832,-3.);
#9124=DERIVED_UNIT_ELEMENT(#9128,1.);
#9125=DERIVED_UNIT_ELEMENT(#17832,-3.);
#9126=DERIVED_UNIT_ELEMENT(#9128,1.);
#9127=DERIVED_UNIT_ELEMENT(#17832,-3.);
#9128=(
MASS_UNIT()
NAMED_UNIT(*)
SI_UNIT(.KILO.,.GRAM.)
);
#9129=DERIVED_UNIT((#9042,#9043));
#9130=DERIVED_UNIT((#9044,#9045));
#9131=DERIVED_UNIT((#9046,#9047));
#9132=DERIVED_UNIT((#9048,#9049));
#9133=DERIVED_UNIT((#9050,#9051));
#9134=DERIVED_UNIT((#9052,#9053));
#9135=DERIVED_UNIT((#9054,#9055));
#9136=DERIVED_UNIT((#9056,#9057));
#9137=DERIVED_UNIT((#9058,#9059));
#9138=DERIVED_UNIT((#9060,#9061));
#9139=DERIVED_UNIT((#9062,#9063));
#9140=DERIVED_UNIT((#9064,#9065));
#9141=DERIVED_UNIT((#9066,#9067));
#9142=DERIVED_UNIT((#9068,#9069));
#9143=DERIVED_UNIT((#9070,#9071));
#9144=DERIVED_UNIT((#9072,#9073));
#9145=DERIVED_UNIT((#9074,#9075));
#9146=DERIVED_UNIT((#9076,#9077));
#9147=DERIVED_UNIT((#9078,#9079));
#9148=DERIVED_UNIT((#9080,#9081));
#9149=DERIVED_UNIT((#9082,#9083));
#9150=DERIVED_UNIT((#9084,#9085));
#9151=DERIVED_UNIT((#9086,#9087));
#9152=DERIVED_UNIT((#9088,#9089));
#9153=DERIVED_UNIT((#9090,#9091));
#9154=DERIVED_UNIT((#9092,#9093));
#9155=DERIVED_UNIT((#9094,#9095));
#9156=DERIVED_UNIT((#9096,#9097));
#9157=DERIVED_UNIT((#9098,#9099));
#9158=DERIVED_UNIT((#9100,#9101));
#9159=DERIVED_UNIT((#9102,#9103));
#9160=DERIVED_UNIT((#9104,#9105));
#9161=DERIVED_UNIT((#9106,#9107));
#9162=DERIVED_UNIT((#9108,#9109));
#9163=DERIVED_UNIT((#9110,#9111));
#9164=DERIVED_UNIT((#9112,#9113));
#9165=DERIVED_UNIT((#9114,#9115));
#9166=DERIVED_UNIT((#9116,#9117));
#9167=DERIVED_UNIT((#9118,#9119));
#9168=DERIVED_UNIT((#9120,#9121));
#9169=DERIVED_UNIT((#9122,#9123));
#9170=DERIVED_UNIT((#9124,#9125));
#9171=DERIVED_UNIT((#9126,#9127));
#9172=MEASURE_REPRESENTATION_ITEM('density measure',
POSITIVE_RATIO_MEASURE(7850.),#9129);
#9173=MEASURE_REPRESENTATION_ITEM('density measure',
POSITIVE_RATIO_MEASURE(7850.),#9130);
#9174=MEASURE_REPRESENTATION_ITEM('density measure',
POSITIVE_RATIO_MEASURE(7850.),#9131);
#9175=MEASURE_REPRESENTATION_ITEM('density measure',
POSITIVE_RATIO_MEASURE(7850.),#9132);
#9176=MEASURE_REPRESENTATION_ITEM('density measure',
POSITIVE_RATIO_MEASURE(7850.),#9133);
#9177=MEASURE_REPRESENTATION_ITEM('density measure',
POSITIVE_RATIO_MEASURE(7850.),#9134);
#9178=MEASURE_REPRESENTATION_ITEM('density measure',
POSITIVE_RATIO_MEASURE(7850.),#9135);
#9179=MEASURE_REPRESENTATION_ITEM('density measure',
POSITIVE_RATIO_MEASURE(7850.),#9136);
#9180=MEASURE_REPRESENTATION_ITEM('density measure',
POSITIVE_RATIO_MEASURE(7850.),#9137);
#9181=MEASURE_REPRESENTATION_ITEM('density measure',
POSITIVE_RATIO_MEASURE(7850.),#9138);
#9182=MEASURE_REPRESENTATION_ITEM('density measure',
POSITIVE_RATIO_MEASURE(7850.),#9139);
#9183=MEASURE_REPRESENTATION_ITEM('density measure',
POSITIVE_RATIO_MEASURE(7850.),#9140);
#9184=MEASURE_REPRESENTATION_ITEM('density measure',
POSITIVE_RATIO_MEASURE(7850.),#9141);
#9185=MEASURE_REPRESENTATION_ITEM('density measure',
POSITIVE_RATIO_MEASURE(7850.),#9142);
#9186=MEASURE_REPRESENTATION_ITEM('density measure',
POSITIVE_RATIO_MEASURE(7850.),#9143);
#9187=MEASURE_REPRESENTATION_ITEM('density measure',
POSITIVE_RATIO_MEASURE(7850.),#9144);
#9188=MEASURE_REPRESENTATION_ITEM('density measure',
POSITIVE_RATIO_MEASURE(7850.),#9145);
#9189=MEASURE_REPRESENTATION_ITEM('density measure',
POSITIVE_RATIO_MEASURE(7850.),#9146);
#9190=MEASURE_REPRESENTATION_ITEM('density measure',
POSITIVE_RATIO_MEASURE(7850.),#9147);
#9191=MEASURE_REPRESENTATION_ITEM('density measure',
POSITIVE_RATIO_MEASURE(7850.),#9148);
#9192=MEASURE_REPRESENTATION_ITEM('density measure',
POSITIVE_RATIO_MEASURE(7850.),#9149);
#9193=MEASURE_REPRESENTATION_ITEM('density measure',
POSITIVE_RATIO_MEASURE(7850.),#9150);
#9194=MEASURE_REPRESENTATION_ITEM('density measure',
POSITIVE_RATIO_MEASURE(7850.),#9151);
#9195=MEASURE_REPRESENTATION_ITEM('density measure',
POSITIVE_RATIO_MEASURE(7850.),#9152);
#9196=MEASURE_REPRESENTATION_ITEM('density measure',
POSITIVE_RATIO_MEASURE(7850.),#9153);
#9197=MEASURE_REPRESENTATION_ITEM('density measure',
POSITIVE_RATIO_MEASURE(7850.),#9154);
#9198=MEASURE_REPRESENTATION_ITEM('density measure',
POSITIVE_RATIO_MEASURE(7850.),#9155);
#9199=MEASURE_REPRESENTATION_ITEM('density measure',
POSITIVE_RATIO_MEASURE(7850.),#9156);
#9200=MEASURE_REPRESENTATION_ITEM('density measure',
POSITIVE_RATIO_MEASURE(7850.),#9157);
#9201=MEASURE_REPRESENTATION_ITEM('density measure',
POSITIVE_RATIO_MEASURE(7850.),#9158);
#9202=MEASURE_REPRESENTATION_ITEM('density measure',
POSITIVE_RATIO_MEASURE(7850.),#9159);
#9203=MEASURE_REPRESENTATION_ITEM('density measure',
POSITIVE_RATIO_MEASURE(7850.),#9160);
#9204=MEASURE_REPRESENTATION_ITEM('density measure',
POSITIVE_RATIO_MEASURE(7850.),#9161);
#9205=MEASURE_REPRESENTATION_ITEM('density measure',
POSITIVE_RATIO_MEASURE(7850.),#9162);
#9206=MEASURE_REPRESENTATION_ITEM('density measure',
POSITIVE_RATIO_MEASURE(7850.),#9163);
#9207=MEASURE_REPRESENTATION_ITEM('density measure',
POSITIVE_RATIO_MEASURE(7850.),#9164);
#9208=MEASURE_REPRESENTATION_ITEM('density measure',
POSITIVE_RATIO_MEASURE(7850.),#9165);
#9209=MEASURE_REPRESENTATION_ITEM('density measure',
POSITIVE_RATIO_MEASURE(7850.),#9166);
#9210=MEASURE_REPRESENTATION_ITEM('density measure',
POSITIVE_RATIO_MEASURE(7850.),#9167);
#9211=MEASURE_REPRESENTATION_ITEM('density measure',
POSITIVE_RATIO_MEASURE(7850.),#9168);
#9212=MEASURE_REPRESENTATION_ITEM('density measure',
POSITIVE_RATIO_MEASURE(7850.),#9169);
#9213=MEASURE_REPRESENTATION_ITEM('density measure',
POSITIVE_RATIO_MEASURE(7850.),#9170);
#9214=MEASURE_REPRESENTATION_ITEM('density measure',
POSITIVE_RATIO_MEASURE(7850.),#9171);
#9215=PROPERTY_DEFINITION_REPRESENTATION(#9430,#9301);
#9216=PROPERTY_DEFINITION_REPRESENTATION(#9431,#9302);
#9217=PROPERTY_DEFINITION_REPRESENTATION(#9432,#9303);
#9218=PROPERTY_DEFINITION_REPRESENTATION(#9433,#9304);
#9219=PROPERTY_DEFINITION_REPRESENTATION(#9434,#9305);
#9220=PROPERTY_DEFINITION_REPRESENTATION(#9435,#9306);
#9221=PROPERTY_DEFINITION_REPRESENTATION(#9436,#9307);
#9222=PROPERTY_DEFINITION_REPRESENTATION(#9437,#9308);
#9223=PROPERTY_DEFINITION_REPRESENTATION(#9438,#9309);
#9224=PROPERTY_DEFINITION_REPRESENTATION(#9439,#9310);
#9225=PROPERTY_DEFINITION_REPRESENTATION(#9440,#9311);
#9226=PROPERTY_DEFINITION_REPRESENTATION(#9441,#9312);
#9227=PROPERTY_DEFINITION_REPRESENTATION(#9442,#9313);
#9228=PROPERTY_DEFINITION_REPRESENTATION(#9443,#9314);
#9229=PROPERTY_DEFINITION_REPRESENTATION(#9444,#9315);
#9230=PROPERTY_DEFINITION_REPRESENTATION(#9445,#9316);
#9231=PROPERTY_DEFINITION_REPRESENTATION(#9446,#9317);
#9232=PROPERTY_DEFINITION_REPRESENTATION(#9447,#9318);
#9233=PROPERTY_DEFINITION_REPRESENTATION(#9448,#9319);
#9234=PROPERTY_DEFINITION_REPRESENTATION(#9449,#9320);
#9235=PROPERTY_DEFINITION_REPRESENTATION(#9450,#9321);
#9236=PROPERTY_DEFINITION_REPRESENTATION(#9451,#9322);
#9237=PROPERTY_DEFINITION_REPRESENTATION(#9452,#9323);
#9238=PROPERTY_DEFINITION_REPRESENTATION(#9453,#9324);
#9239=PROPERTY_DEFINITION_REPRESENTATION(#9454,#9325);
#9240=PROPERTY_DEFINITION_REPRESENTATION(#9455,#9326);
#9241=PROPERTY_DEFINITION_REPRESENTATION(#9456,#9327);
#9242=PROPERTY_DEFINITION_REPRESENTATION(#9457,#9328);
#9243=PROPERTY_DEFINITION_REPRESENTATION(#9458,#9329);
#9244=PROPERTY_DEFINITION_REPRESENTATION(#9459,#9330);
#9245=PROPERTY_DEFINITION_REPRESENTATION(#9460,#9331);
#9246=PROPERTY_DEFINITION_REPRESENTATION(#9461,#9332);
#9247=PROPERTY_DEFINITION_REPRESENTATION(#9462,#9333);
#9248=PROPERTY_DEFINITION_REPRESENTATION(#9463,#9334);
#9249=PROPERTY_DEFINITION_REPRESENTATION(#9464,#9335);
#9250=PROPERTY_DEFINITION_REPRESENTATION(#9465,#9336);
#9251=PROPERTY_DEFINITION_REPRESENTATION(#9466,#9337);
#9252=PROPERTY_DEFINITION_REPRESENTATION(#9467,#9338);
#9253=PROPERTY_DEFINITION_REPRESENTATION(#9468,#9339);
#9254=PROPERTY_DEFINITION_REPRESENTATION(#9469,#9340);
#9255=PROPERTY_DEFINITION_REPRESENTATION(#9470,#9341);
#9256=PROPERTY_DEFINITION_REPRESENTATION(#9471,#9342);
#9257=PROPERTY_DEFINITION_REPRESENTATION(#9472,#9343);
#9258=PROPERTY_DEFINITION_REPRESENTATION(#9473,#9344);
#9259=PROPERTY_DEFINITION_REPRESENTATION(#9474,#9345);
#9260=PROPERTY_DEFINITION_REPRESENTATION(#9475,#9346);
#9261=PROPERTY_DEFINITION_REPRESENTATION(#9476,#9347);
#9262=PROPERTY_DEFINITION_REPRESENTATION(#9477,#9348);
#9263=PROPERTY_DEFINITION_REPRESENTATION(#9478,#9349);
#9264=PROPERTY_DEFINITION_REPRESENTATION(#9479,#9350);
#9265=PROPERTY_DEFINITION_REPRESENTATION(#9480,#9351);
#9266=PROPERTY_DEFINITION_REPRESENTATION(#9481,#9352);
#9267=PROPERTY_DEFINITION_REPRESENTATION(#9482,#9353);
#9268=PROPERTY_DEFINITION_REPRESENTATION(#9483,#9354);
#9269=PROPERTY_DEFINITION_REPRESENTATION(#9484,#9355);
#9270=PROPERTY_DEFINITION_REPRESENTATION(#9485,#9356);
#9271=PROPERTY_DEFINITION_REPRESENTATION(#9486,#9357);
#9272=PROPERTY_DEFINITION_REPRESENTATION(#9487,#9358);
#9273=PROPERTY_DEFINITION_REPRESENTATION(#9488,#9359);
#9274=PROPERTY_DEFINITION_REPRESENTATION(#9489,#9360);
#9275=PROPERTY_DEFINITION_REPRESENTATION(#9490,#9361);
#9276=PROPERTY_DEFINITION_REPRESENTATION(#9491,#9362);
#9277=PROPERTY_DEFINITION_REPRESENTATION(#9492,#9363);
#9278=PROPERTY_DEFINITION_REPRESENTATION(#9493,#9364);
#9279=PROPERTY_DEFINITION_REPRESENTATION(#9494,#9365);
#9280=PROPERTY_DEFINITION_REPRESENTATION(#9495,#9366);
#9281=PROPERTY_DEFINITION_REPRESENTATION(#9496,#9367);
#9282=PROPERTY_DEFINITION_REPRESENTATION(#9497,#9368);
#9283=PROPERTY_DEFINITION_REPRESENTATION(#9498,#9369);
#9284=PROPERTY_DEFINITION_REPRESENTATION(#9499,#9370);
#9285=PROPERTY_DEFINITION_REPRESENTATION(#9500,#9371);
#9286=PROPERTY_DEFINITION_REPRESENTATION(#9501,#9372);
#9287=PROPERTY_DEFINITION_REPRESENTATION(#9502,#9373);
#9288=PROPERTY_DEFINITION_REPRESENTATION(#9503,#9374);
#9289=PROPERTY_DEFINITION_REPRESENTATION(#9504,#9375);
#9290=PROPERTY_DEFINITION_REPRESENTATION(#9505,#9376);
#9291=PROPERTY_DEFINITION_REPRESENTATION(#9506,#9377);
#9292=PROPERTY_DEFINITION_REPRESENTATION(#9507,#9378);
#9293=PROPERTY_DEFINITION_REPRESENTATION(#9508,#9379);
#9294=PROPERTY_DEFINITION_REPRESENTATION(#9509,#9380);
#9295=PROPERTY_DEFINITION_REPRESENTATION(#9510,#9381);
#9296=PROPERTY_DEFINITION_REPRESENTATION(#9511,#9382);
#9297=PROPERTY_DEFINITION_REPRESENTATION(#9512,#9383);
#9298=PROPERTY_DEFINITION_REPRESENTATION(#9513,#9384);
#9299=PROPERTY_DEFINITION_REPRESENTATION(#9514,#9385);
#9300=PROPERTY_DEFINITION_REPRESENTATION(#9515,#9386);
#9301=REPRESENTATION('material name',(#9387),#17783);
#9302=REPRESENTATION('density',(#9172),#17783);
#9303=REPRESENTATION('material name',(#9388),#17784);
#9304=REPRESENTATION('density',(#9173),#17784);
#9305=REPRESENTATION('material name',(#9389),#17785);
#9306=REPRESENTATION('density',(#9174),#17785);
#9307=REPRESENTATION('material name',(#9390),#17786);
#9308=REPRESENTATION('density',(#9175),#17786);
#9309=REPRESENTATION('material name',(#9391),#17787);
#9310=REPRESENTATION('density',(#9176),#17787);
#9311=REPRESENTATION('material name',(#9392),#17788);
#9312=REPRESENTATION('density',(#9177),#17788);
#9313=REPRESENTATION('material name',(#9393),#17789);
#9314=REPRESENTATION('density',(#9178),#17789);
#9315=REPRESENTATION('material name',(#9394),#17790);
#9316=REPRESENTATION('density',(#9179),#17790);
#9317=REPRESENTATION('material name',(#9395),#17791);
#9318=REPRESENTATION('density',(#9180),#17791);
#9319=REPRESENTATION('material name',(#9396),#17792);
#9320=REPRESENTATION('density',(#9181),#17792);
#9321=REPRESENTATION('material name',(#9397),#17793);
#9322=REPRESENTATION('density',(#9182),#17793);
#9323=REPRESENTATION('material name',(#9398),#17794);
#9324=REPRESENTATION('density',(#9183),#17794);
#9325=REPRESENTATION('material name',(#9399),#17795);
#9326=REPRESENTATION('density',(#9184),#17795);
#9327=REPRESENTATION('material name',(#9400),#17796);
#9328=REPRESENTATION('density',(#9185),#17796);
#9329=REPRESENTATION('material name',(#9401),#17797);
#9330=REPRESENTATION('density',(#9186),#17797);
#9331=REPRESENTATION('material name',(#9402),#17798);
#9332=REPRESENTATION('density',(#9187),#17798);
#9333=REPRESENTATION('material name',(#9403),#17800);
#9334=REPRESENTATION('density',(#9188),#17800);
#9335=REPRESENTATION('material name',(#9404),#17801);
#9336=REPRESENTATION('density',(#9189),#17801);
#9337=REPRESENTATION('material name',(#9405),#17802);
#9338=REPRESENTATION('density',(#9190),#17802);
#9339=REPRESENTATION('material name',(#9406),#17803);
#9340=REPRESENTATION('density',(#9191),#17803);
#9341=REPRESENTATION('material name',(#9407),#17804);
#9342=REPRESENTATION('density',(#9192),#17804);
#9343=REPRESENTATION('material name',(#9408),#17805);
#9344=REPRESENTATION('density',(#9193),#17805);
#9345=REPRESENTATION('material name',(#9409),#17807);
#9346=REPRESENTATION('density',(#9194),#17807);
#9347=REPRESENTATION('material name',(#9410),#17808);
#9348=REPRESENTATION('density',(#9195),#17808);
#9349=REPRESENTATION('material name',(#9411),#17809);
#9350=REPRESENTATION('density',(#9196),#17809);
#9351=REPRESENTATION('material name',(#9412),#17810);
#9352=REPRESENTATION('density',(#9197),#17810);
#9353=REPRESENTATION('material name',(#9413),#17811);
#9354=REPRESENTATION('density',(#9198),#17811);
#9355=REPRESENTATION('material name',(#9414),#17812);
#9356=REPRESENTATION('density',(#9199),#17812);
#9357=REPRESENTATION('material name',(#9415),#17814);
#9358=REPRESENTATION('density',(#9200),#17814);
#9359=REPRESENTATION('material name',(#9416),#17815);
#9360=REPRESENTATION('density',(#9201),#17815);
#9361=REPRESENTATION('material name',(#9417),#17816);
#9362=REPRESENTATION('density',(#9202),#17816);
#9363=REPRESENTATION('material name',(#9418),#17817);
#9364=REPRESENTATION('density',(#9203),#17817);
#9365=REPRESENTATION('material name',(#9419),#17818);
#9366=REPRESENTATION('density',(#9204),#17818);
#9367=REPRESENTATION('material name',(#9420),#17819);
#9368=REPRESENTATION('density',(#9205),#17819);
#9369=REPRESENTATION('material name',(#9421),#17820);
#9370=REPRESENTATION('density',(#9206),#17820);
#9371=REPRESENTATION('material name',(#9422),#17822);
#9372=REPRESENTATION('density',(#9207),#17822);
#9373=REPRESENTATION('material name',(#9423),#17823);
#9374=REPRESENTATION('density',(#9208),#17823);
#9375=REPRESENTATION('material name',(#9424),#17824);
#9376=REPRESENTATION('density',(#9209),#17824);
#9377=REPRESENTATION('material name',(#9425),#17825);
#9378=REPRESENTATION('density',(#9210),#17825);
#9379=REPRESENTATION('material name',(#9426),#17826);
#9380=REPRESENTATION('density',(#9211),#17826);
#9381=REPRESENTATION('material name',(#9427),#17827);
#9382=REPRESENTATION('density',(#9212),#17827);
#9383=REPRESENTATION('material name',(#9428),#17828);
#9384=REPRESENTATION('density',(#9213),#17828);
#9385=REPRESENTATION('material name',(#9429),#17829);
#9386=REPRESENTATION('density',(#9214),#17829);
#9387=DESCRIPTIVE_REPRESENTATION_ITEM('Steel','Steel');
#9388=DESCRIPTIVE_REPRESENTATION_ITEM('Steel','Steel');
#9389=DESCRIPTIVE_REPRESENTATION_ITEM('Steel','Steel');
#9390=DESCRIPTIVE_REPRESENTATION_ITEM('Steel','Steel');
#9391=DESCRIPTIVE_REPRESENTATION_ITEM('Steel','Steel');
#9392=DESCRIPTIVE_REPRESENTATION_ITEM('Steel','Steel');
#9393=DESCRIPTIVE_REPRESENTATION_ITEM('Steel','Steel');
#9394=DESCRIPTIVE_REPRESENTATION_ITEM('Steel','Steel');
#9395=DESCRIPTIVE_REPRESENTATION_ITEM('Steel','Steel');
#9396=DESCRIPTIVE_REPRESENTATION_ITEM('Steel','Steel');
#9397=DESCRIPTIVE_REPRESENTATION_ITEM('Steel','Steel');
#9398=DESCRIPTIVE_REPRESENTATION_ITEM('Steel','Steel');
#9399=DESCRIPTIVE_REPRESENTATION_ITEM('Steel','Steel');
#9400=DESCRIPTIVE_REPRESENTATION_ITEM('Steel','Steel');
#9401=DESCRIPTIVE_REPRESENTATION_ITEM('Steel','Steel');
#9402=DESCRIPTIVE_REPRESENTATION_ITEM('Steel','Steel');
#9403=DESCRIPTIVE_REPRESENTATION_ITEM('Steel','Steel');
#9404=DESCRIPTIVE_REPRESENTATION_ITEM('Steel','Steel');
#9405=DESCRIPTIVE_REPRESENTATION_ITEM('Steel','Steel');
#9406=DESCRIPTIVE_REPRESENTATION_ITEM('Steel','Steel');
#9407=DESCRIPTIVE_REPRESENTATION_ITEM('Steel','Steel');
#9408=DESCRIPTIVE_REPRESENTATION_ITEM('Steel','Steel');
#9409=DESCRIPTIVE_REPRESENTATION_ITEM('Steel','Steel');
#9410=DESCRIPTIVE_REPRESENTATION_ITEM('Steel','Steel');
#9411=DESCRIPTIVE_REPRESENTATION_ITEM('Steel','Steel');
#9412=DESCRIPTIVE_REPRESENTATION_ITEM('Steel','Steel');
#9413=DESCRIPTIVE_REPRESENTATION_ITEM('Steel','Steel');
#9414=DESCRIPTIVE_REPRESENTATION_ITEM('Steel','Steel');
#9415=DESCRIPTIVE_REPRESENTATION_ITEM('Steel','Steel');
#9416=DESCRIPTIVE_REPRESENTATION_ITEM('Steel','Steel');
#9417=DESCRIPTIVE_REPRESENTATION_ITEM('Steel','Steel');
#9418=DESCRIPTIVE_REPRESENTATION_ITEM('Steel','Steel');
#9419=DESCRIPTIVE_REPRESENTATION_ITEM('Steel','Steel');
#9420=DESCRIPTIVE_REPRESENTATION_ITEM('Steel','Steel');
#9421=DESCRIPTIVE_REPRESENTATION_ITEM('Steel','Steel');
#9422=DESCRIPTIVE_REPRESENTATION_ITEM('Steel','Steel');
#9423=DESCRIPTIVE_REPRESENTATION_ITEM('Steel','Steel');
#9424=DESCRIPTIVE_REPRESENTATION_ITEM('Steel','Steel');
#9425=DESCRIPTIVE_REPRESENTATION_ITEM('Steel','Steel');
#9426=DESCRIPTIVE_REPRESENTATION_ITEM('Steel','Steel');
#9427=DESCRIPTIVE_REPRESENTATION_ITEM('Steel','Steel');
#9428=DESCRIPTIVE_REPRESENTATION_ITEM('Steel','Steel');
#9429=DESCRIPTIVE_REPRESENTATION_ITEM('Steel','Steel');
#9430=PROPERTY_DEFINITION('material property','material name',#18058);
#9431=PROPERTY_DEFINITION('material property','density of part',#18058);
#9432=PROPERTY_DEFINITION('material property','material name',#18059);
#9433=PROPERTY_DEFINITION('material property','density of part',#18059);
#9434=PROPERTY_DEFINITION('material property','material name',#18060);
#9435=PROPERTY_DEFINITION('material property','density of part',#18060);
#9436=PROPERTY_DEFINITION('material property','material name',#18061);
#9437=PROPERTY_DEFINITION('material property','density of part',#18061);
#9438=PROPERTY_DEFINITION('material property','material name',#18062);
#9439=PROPERTY_DEFINITION('material property','density of part',#18062);
#9440=PROPERTY_DEFINITION('material property','material name',#18063);
#9441=PROPERTY_DEFINITION('material property','density of part',#18063);
#9442=PROPERTY_DEFINITION('material property','material name',#18064);
#9443=PROPERTY_DEFINITION('material property','density of part',#18064);
#9444=PROPERTY_DEFINITION('material property','material name',#18065);
#9445=PROPERTY_DEFINITION('material property','density of part',#18065);
#9446=PROPERTY_DEFINITION('material property','material name',#18066);
#9447=PROPERTY_DEFINITION('material property','density of part',#18066);
#9448=PROPERTY_DEFINITION('material property','material name',#18067);
#9449=PROPERTY_DEFINITION('material property','density of part',#18067);
#9450=PROPERTY_DEFINITION('material property','material name',#18068);
#9451=PROPERTY_DEFINITION('material property','density of part',#18068);
#9452=PROPERTY_DEFINITION('material property','material name',#18069);
#9453=PROPERTY_DEFINITION('material property','density of part',#18069);
#9454=PROPERTY_DEFINITION('material property','material name',#18070);
#9455=PROPERTY_DEFINITION('material property','density of part',#18070);
#9456=PROPERTY_DEFINITION('material property','material name',#18071);
#9457=PROPERTY_DEFINITION('material property','density of part',#18071);
#9458=PROPERTY_DEFINITION('material property','material name',#18072);
#9459=PROPERTY_DEFINITION('material property','density of part',#18072);
#9460=PROPERTY_DEFINITION('material property','material name',#18073);
#9461=PROPERTY_DEFINITION('material property','density of part',#18073);
#9462=PROPERTY_DEFINITION('material property','material name',#18075);
#9463=PROPERTY_DEFINITION('material property','density of part',#18075);
#9464=PROPERTY_DEFINITION('material property','material name',#18076);
#9465=PROPERTY_DEFINITION('material property','density of part',#18076);
#9466=PROPERTY_DEFINITION('material property','material name',#18077);
#9467=PROPERTY_DEFINITION('material property','density of part',#18077);
#9468=PROPERTY_DEFINITION('material property','material name',#18078);
#9469=PROPERTY_DEFINITION('material property','density of part',#18078);
#9470=PROPERTY_DEFINITION('material property','material name',#18079);
#9471=PROPERTY_DEFINITION('material property','density of part',#18079);
#9472=PROPERTY_DEFINITION('material property','material name',#18080);
#9473=PROPERTY_DEFINITION('material property','density of part',#18080);
#9474=PROPERTY_DEFINITION('material property','material name',#18082);
#9475=PROPERTY_DEFINITION('material property','density of part',#18082);
#9476=PROPERTY_DEFINITION('material property','material name',#18083);
#9477=PROPERTY_DEFINITION('material property','density of part',#18083);
#9478=PROPERTY_DEFINITION('material property','material name',#18084);
#9479=PROPERTY_DEFINITION('material property','density of part',#18084);
#9480=PROPERTY_DEFINITION('material property','material name',#18085);
#9481=PROPERTY_DEFINITION('material property','density of part',#18085);
#9482=PROPERTY_DEFINITION('material property','material name',#18086);
#9483=PROPERTY_DEFINITION('material property','density of part',#18086);
#9484=PROPERTY_DEFINITION('material property','material name',#18087);
#9485=PROPERTY_DEFINITION('material property','density of part',#18087);
#9486=PROPERTY_DEFINITION('material property','material name',#18089);
#9487=PROPERTY_DEFINITION('material property','density of part',#18089);
#9488=PROPERTY_DEFINITION('material property','material name',#18090);
#9489=PROPERTY_DEFINITION('material property','density of part',#18090);
#9490=PROPERTY_DEFINITION('material property','material name',#18091);
#9491=PROPERTY_DEFINITION('material property','density of part',#18091);
#9492=PROPERTY_DEFINITION('material property','material name',#18092);
#9493=PROPERTY_DEFINITION('material property','density of part',#18092);
#9494=PROPERTY_DEFINITION('material property','material name',#18093);
#9495=PROPERTY_DEFINITION('material property','density of part',#18093);
#9496=PROPERTY_DEFINITION('material property','material name',#18094);
#9497=PROPERTY_DEFINITION('material property','density of part',#18094);
#9498=PROPERTY_DEFINITION('material property','material name',#18095);
#9499=PROPERTY_DEFINITION('material property','density of part',#18095);
#9500=PROPERTY_DEFINITION('material property','material name',#18097);
#9501=PROPERTY_DEFINITION('material property','density of part',#18097);
#9502=PROPERTY_DEFINITION('material property','material name',#18098);
#9503=PROPERTY_DEFINITION('material property','density of part',#18098);
#9504=PROPERTY_DEFINITION('material property','material name',#18099);
#9505=PROPERTY_DEFINITION('material property','density of part',#18099);
#9506=PROPERTY_DEFINITION('material property','material name',#18100);
#9507=PROPERTY_DEFINITION('material property','density of part',#18100);
#9508=PROPERTY_DEFINITION('material property','material name',#18101);
#9509=PROPERTY_DEFINITION('material property','density of part',#18101);
#9510=PROPERTY_DEFINITION('material property','material name',#18102);
#9511=PROPERTY_DEFINITION('material property','density of part',#18102);
#9512=PROPERTY_DEFINITION('material property','material name',#18103);
#9513=PROPERTY_DEFINITION('material property','density of part',#18103);
#9514=PROPERTY_DEFINITION('material property','material name',#18104);
#9515=PROPERTY_DEFINITION('material property','density of part',#18104);
#9516=AXIS2_PLACEMENT_3D('',#13873,#10809,#10810);
#9517=AXIS2_PLACEMENT_3D('',#13874,#10811,#10812);
#9518=AXIS2_PLACEMENT_3D('',#13875,#10813,#10814);
#9519=AXIS2_PLACEMENT_3D('',#13876,#10815,#10816);
#9520=AXIS2_PLACEMENT_3D('',#13881,#10818,#10819);
#9521=AXIS2_PLACEMENT_3D('',#13884,#10821,#10822);
#9522=AXIS2_PLACEMENT_3D('',#13885,#10823,#10824);
#9523=AXIS2_PLACEMENT_3D('',#13890,#10826,#10827);
#9524=AXIS2_PLACEMENT_3D('',#13893,#10829,#10830);
#9525=AXIS2_PLACEMENT_3D('',#13894,#10831,#10832);
#9526=AXIS2_PLACEMENT_3D('',#13905,#10837,#10838);
#9527=AXIS2_PLACEMENT_3D('',#13909,#10840,#10841);
#9528=AXIS2_PLACEMENT_3D('',#13913,#10843,#10844);
#9529=AXIS2_PLACEMENT_3D('',#13917,#10846,#10847);
#9530=AXIS2_PLACEMENT_3D('',#13921,#10849,#10850);
#9531=AXIS2_PLACEMENT_3D('',#13925,#10852,#10853);
#9532=AXIS2_PLACEMENT_3D('',#13929,#10857,#10858);
#9533=AXIS2_PLACEMENT_3D('',#13931,#10860,#10861);
#9534=AXIS2_PLACEMENT_3D('',#13933,#10863,#10864);
#9535=AXIS2_PLACEMENT_3D('',#13938,#10867,#10868);
#9536=AXIS2_PLACEMENT_3D('',#13939,#10869,#10870);
#9537=AXIS2_PLACEMENT_3D('',#13943,#10872,#10873);
#9538=AXIS2_PLACEMENT_3D('',#13945,#10875,#10876);
#9539=AXIS2_PLACEMENT_3D('',#13947,#10878,#10879);
#9540=AXIS2_PLACEMENT_3D('',#13949,#10881,#10882);
#9541=AXIS2_PLACEMENT_3D('',#13954,#10884,#10885);
#9542=AXIS2_PLACEMENT_3D('',#13959,#10888,#10889);
#9543=AXIS2_PLACEMENT_3D('',#13962,#10891,#10892);
#9544=AXIS2_PLACEMENT_3D('',#13963,#10893,#10894);
#9545=AXIS2_PLACEMENT_3D('',#13967,#10896,#10897);
#9546=AXIS2_PLACEMENT_3D('',#13969,#10899,#10900);
#9547=AXIS2_PLACEMENT_3D('',#13971,#10902,#10903);
#9548=AXIS2_PLACEMENT_3D('',#13973,#10905,#10906);
#9549=AXIS2_PLACEMENT_3D('',#13978,#10908,#10909);
#9550=AXIS2_PLACEMENT_3D('',#13983,#10912,#10913);
#9551=AXIS2_PLACEMENT_3D('',#13986,#10915,#10916);
#9552=AXIS2_PLACEMENT_3D('',#13987,#10917,#10918);
#9553=AXIS2_PLACEMENT_3D('',#13991,#10920,#10921);
#9554=AXIS2_PLACEMENT_3D('',#13993,#10923,#10924);
#9555=AXIS2_PLACEMENT_3D('',#13995,#10926,#10927);
#9556=AXIS2_PLACEMENT_3D('',#13997,#10929,#10930);
#9557=AXIS2_PLACEMENT_3D('',#13998,#10931,#10932);
#9558=AXIS2_PLACEMENT_3D('',#13999,#10933,#10934);
#9559=AXIS2_PLACEMENT_3D('',#14000,#10935,#10936);
#9560=AXIS2_PLACEMENT_3D('',#14001,#10937,#10938);
#9561=AXIS2_PLACEMENT_3D('',#14003,#10939,#10940);
#9562=AXIS2_PLACEMENT_3D('',#14006,#10942,#10943);
#9563=AXIS2_PLACEMENT_3D('',#14007,#10944,#10945);
#9564=AXIS2_PLACEMENT_3D('',#14008,#10946,#10947);
#9565=AXIS2_PLACEMENT_3D('',#14010,#10948,#10949);
#9566=AXIS2_PLACEMENT_3D('',#14013,#10951,#10952);
#9567=AXIS2_PLACEMENT_3D('',#14014,#10953,#10954);
#9568=AXIS2_PLACEMENT_3D('',#14015,#10955,#10956);
#9569=AXIS2_PLACEMENT_3D('',#14016,#10957,#10958);
#9570=AXIS2_PLACEMENT_3D('',#14017,#10959,#10960);
#9571=AXIS2_PLACEMENT_3D('',#14018,#10961,#10962);
#9572=AXIS2_PLACEMENT_3D('',#14019,#10963,#10964);
#9573=AXIS2_PLACEMENT_3D('',#14025,#10968,#10969);
#9574=AXIS2_PLACEMENT_3D('',#14029,#10972,#10973);
#9575=AXIS2_PLACEMENT_3D('',#14033,#10976,#10977);
#9576=AXIS2_PLACEMENT_3D('',#14035,#10979,#10980);
#9577=AXIS2_PLACEMENT_3D('',#14036,#10981,#10982);
#9578=AXIS2_PLACEMENT_3D('',#14037,#10983,#10984);
#9579=AXIS2_PLACEMENT_3D('',#14046,#10989,#10990);
#9580=AXIS2_PLACEMENT_3D('',#14052,#10994,#10995);
#9581=AXIS2_PLACEMENT_3D('',#14058,#10999,#11000);
#9582=AXIS2_PLACEMENT_3D('',#14061,#11003,#11004);
#9583=AXIS2_PLACEMENT_3D('',#14062,#11005,#11006);
#9584=AXIS2_PLACEMENT_3D('',#14063,#11007,#11008);
#9585=AXIS2_PLACEMENT_3D('',#14064,#11009,#11010);
#9586=AXIS2_PLACEMENT_3D('',#14073,#11015,#11016);
#9587=AXIS2_PLACEMENT_3D('',#14079,#11020,#11021);
#9588=AXIS2_PLACEMENT_3D('',#14085,#11025,#11026);
#9589=AXIS2_PLACEMENT_3D('',#14088,#11029,#11030);
#9590=AXIS2_PLACEMENT_3D('',#14089,#11031,#11032);
#9591=AXIS2_PLACEMENT_3D('',#14090,#11033,#11034);
#9592=AXIS2_PLACEMENT_3D('',#14091,#11035,#11036);
#9593=AXIS2_PLACEMENT_3D('',#14093,#11037,#11038);
#9594=AXIS2_PLACEMENT_3D('',#14096,#11040,#11041);
#9595=AXIS2_PLACEMENT_3D('',#14097,#11042,#11043);
#9596=AXIS2_PLACEMENT_3D('',#14099,#11044,#11045);
#9597=AXIS2_PLACEMENT_3D('',#14102,#11047,#11048);
#9598=AXIS2_PLACEMENT_3D('',#14103,#11049,#11050);
#9599=AXIS2_PLACEMENT_3D('',#14105,#11051,#11052);
#9600=AXIS2_PLACEMENT_3D('',#14108,#11054,#11055);
#9601=AXIS2_PLACEMENT_3D('',#14109,#11056,#11057);
#9602=AXIS2_PLACEMENT_3D('',#14111,#11058,#11059);
#9603=AXIS2_PLACEMENT_3D('',#14114,#11061,#11062);
#9604=AXIS2_PLACEMENT_3D('',#14115,#11063,#11064);
#9605=AXIS2_PLACEMENT_3D('',#14117,#11065,#11066);
#9606=AXIS2_PLACEMENT_3D('',#14120,#11068,#11069);
#9607=AXIS2_PLACEMENT_3D('',#14121,#11070,#11071);
#9608=AXIS2_PLACEMENT_3D('',#14123,#11072,#11073);
#9609=AXIS2_PLACEMENT_3D('',#14126,#11075,#11076);
#9610=AXIS2_PLACEMENT_3D('',#14127,#11077,#11078);
#9611=AXIS2_PLACEMENT_3D('',#14129,#11079,#11080);
#9612=AXIS2_PLACEMENT_3D('',#14132,#11082,#11083);
#9613=AXIS2_PLACEMENT_3D('',#14133,#11084,#11085);
#9614=AXIS2_PLACEMENT_3D('',#14135,#11086,#11087);
#9615=AXIS2_PLACEMENT_3D('',#14138,#11089,#11090);
#9616=AXIS2_PLACEMENT_3D('',#14139,#11091,#11092);
#9617=AXIS2_PLACEMENT_3D('',#14141,#11093,#11094);
#9618=AXIS2_PLACEMENT_3D('',#14144,#11096,#11097);
#9619=AXIS2_PLACEMENT_3D('',#14145,#11098,#11099);
#9620=AXIS2_PLACEMENT_3D('',#14154,#11104,#11105);
#9621=AXIS2_PLACEMENT_3D('',#14163,#11110,#11111);
#9622=AXIS2_PLACEMENT_3D('',#14169,#11115,#11116);
#9623=AXIS2_PLACEMENT_3D('',#14175,#11120,#11121);
#9624=AXIS2_PLACEMENT_3D('',#14182,#11126,#11127);
#9625=AXIS2_PLACEMENT_3D('',#14186,#11130,#11131);
#9626=AXIS2_PLACEMENT_3D('',#14191,#11135,#11136);
#9627=AXIS2_PLACEMENT_3D('',#14193,#11138,#11139);
#9628=AXIS2_PLACEMENT_3D('',#14194,#11140,#11141);
#9629=AXIS2_PLACEMENT_3D('',#14195,#11142,#11143);
#9630=AXIS2_PLACEMENT_3D('',#14196,#11144,#11145);
#9631=AXIS2_PLACEMENT_3D('',#14198,#11146,#11147);
#9632=AXIS2_PLACEMENT_3D('',#14201,#11149,#11150);
#9633=AXIS2_PLACEMENT_3D('',#14202,#11151,#11152);
#9634=AXIS2_PLACEMENT_3D('',#14204,#11153,#11154);
#9635=AXIS2_PLACEMENT_3D('',#14207,#11156,#11157);
#9636=AXIS2_PLACEMENT_3D('',#14208,#11158,#11159);
#9637=AXIS2_PLACEMENT_3D('',#14209,#11160,#11161);
#9638=AXIS2_PLACEMENT_3D('',#14210,#11162,#11163);
#9639=AXIS2_PLACEMENT_3D('',#14211,#11164,#11165);
#9640=AXIS2_PLACEMENT_3D('',#14216,#11167,#11168);
#9641=AXIS2_PLACEMENT_3D('',#14219,#11170,#11171);
#9642=AXIS2_PLACEMENT_3D('',#14220,#11172,#11173);
#9643=AXIS2_PLACEMENT_3D('',#14225,#11175,#11176);
#9644=AXIS2_PLACEMENT_3D('',#14228,#11178,#11179);
#9645=AXIS2_PLACEMENT_3D('',#14229,#11180,#11181);
#9646=AXIS2_PLACEMENT_3D('',#14234,#11183,#11184);
#9647=AXIS2_PLACEMENT_3D('',#14237,#11186,#11187);
#9648=AXIS2_PLACEMENT_3D('',#14238,#11188,#11189);
#9649=AXIS2_PLACEMENT_3D('',#14243,#11191,#11192);
#9650=AXIS2_PLACEMENT_3D('',#14246,#11194,#11195);
#9651=AXIS2_PLACEMENT_3D('',#14247,#11196,#11197);
#9652=AXIS2_PLACEMENT_3D('',#14248,#11198,#11199);
#9653=AXIS2_PLACEMENT_3D('',#14249,#11200,#11201);
#9654=AXIS2_PLACEMENT_3D('',#14250,#11202,#11203);
#9655=AXIS2_PLACEMENT_3D('',#14251,#11204,#11205);
#9656=AXIS2_PLACEMENT_3D('',#14253,#11206,#11207);
#9657=AXIS2_PLACEMENT_3D('',#14254,#11208,#11209);
#9658=AXIS2_PLACEMENT_3D('',#14255,#11210,#11211);
#9659=AXIS2_PLACEMENT_3D('',#14256,#11212,#11213);
#9660=AXIS2_PLACEMENT_3D('',#14257,#11214,#11215);
#9661=AXIS2_PLACEMENT_3D('',#14258,#11216,#11217);
#9662=AXIS2_PLACEMENT_3D('',#14259,#11218,#11219);
#9663=AXIS2_PLACEMENT_3D('',#14260,#11220,#11221);
#9664=AXIS2_PLACEMENT_3D('',#14261,#11222,#11223);
#9665=AXIS2_PLACEMENT_3D('',#14262,#11224,#11225);
#9666=AXIS2_PLACEMENT_3D('',#14264,#11226,#11227);
#9667=AXIS2_PLACEMENT_3D('',#14267,#11229,#11230);
#9668=AXIS2_PLACEMENT_3D('',#14268,#11231,#11232);
#9669=AXIS2_PLACEMENT_3D('',#14270,#11233,#11234);
#9670=AXIS2_PLACEMENT_3D('',#14271,#11235,#11236);
#9671=AXIS2_PLACEMENT_3D('',#14273,#11238,#11239);
#9672=AXIS2_PLACEMENT_3D('',#14274,#11240,#11241);
#9673=AXIS2_PLACEMENT_3D('',#14275,#11242,#11243);
#9674=AXIS2_PLACEMENT_3D('',#14280,#11245,#11246);
#9675=AXIS2_PLACEMENT_3D('',#14283,#11248,#11249);
#9676=AXIS2_PLACEMENT_3D('',#14284,#11250,#11251);
#9677=AXIS2_PLACEMENT_3D('',#14289,#11253,#11254);
#9678=AXIS2_PLACEMENT_3D('',#14292,#11256,#11257);
#9679=AXIS2_PLACEMENT_3D('',#14293,#11258,#11259);
#9680=AXIS2_PLACEMENT_3D('',#14298,#11261,#11262);
#9681=AXIS2_PLACEMENT_3D('',#14301,#11264,#11265);
#9682=AXIS2_PLACEMENT_3D('',#14302,#11266,#11267);
#9683=AXIS2_PLACEMENT_3D('',#14307,#11269,#11270);
#9684=AXIS2_PLACEMENT_3D('',#14310,#11272,#11273);
#9685=AXIS2_PLACEMENT_3D('',#14311,#11274,#11275);
#9686=AXIS2_PLACEMENT_3D('',#14312,#11276,#11277);
#9687=AXIS2_PLACEMENT_3D('',#14313,#11278,#11279);
#9688=AXIS2_PLACEMENT_3D('',#14314,#11280,#11281);
#9689=AXIS2_PLACEMENT_3D('',#14315,#11282,#11283);
#9690=AXIS2_PLACEMENT_3D('',#14317,#11284,#11285);
#9691=AXIS2_PLACEMENT_3D('',#14318,#11286,#11287);
#9692=AXIS2_PLACEMENT_3D('',#14319,#11288,#11289);
#9693=AXIS2_PLACEMENT_3D('',#14320,#11290,#11291);
#9694=AXIS2_PLACEMENT_3D('',#14321,#11292,#11293);
#9695=AXIS2_PLACEMENT_3D('',#14322,#11294,#11295);
#9696=AXIS2_PLACEMENT_3D('',#14323,#11296,#11297);
#9697=AXIS2_PLACEMENT_3D('',#14324,#11298,#11299);
#9698=AXIS2_PLACEMENT_3D('',#14325,#11300,#11301);
#9699=AXIS2_PLACEMENT_3D('',#14326,#11302,#11303);
#9700=AXIS2_PLACEMENT_3D('',#14329,#11305,#11306);
#9701=AXIS2_PLACEMENT_3D('',#14330,#11307,#11308);
#9702=AXIS2_PLACEMENT_3D('',#14332,#11309,#11310);
#9703=AXIS2_PLACEMENT_3D('',#14333,#11311,#11312);
#9704=AXIS2_PLACEMENT_3D('',#14335,#11313,#11314);
#9705=AXIS2_PLACEMENT_3D('',#14337,#11316,#11317);
#9706=AXIS2_PLACEMENT_3D('',#14338,#11318,#11319);
#9707=AXIS2_PLACEMENT_3D('',#14339,#11320,#11321);
#9708=AXIS2_PLACEMENT_3D('',#14341,#11322,#11323);
#9709=AXIS2_PLACEMENT_3D('',#14344,#11325,#11326);
#9710=AXIS2_PLACEMENT_3D('',#14345,#11327,#11328);
#9711=AXIS2_PLACEMENT_3D('',#14347,#11329,#11330);
#9712=AXIS2_PLACEMENT_3D('',#14350,#11332,#11333);
#9713=AXIS2_PLACEMENT_3D('',#14351,#11334,#11335);
#9714=AXIS2_PLACEMENT_3D('',#14353,#11336,#11337);
#9715=AXIS2_PLACEMENT_3D('',#14356,#11339,#11340);
#9716=AXIS2_PLACEMENT_3D('',#14357,#11341,#11342);
#9717=AXIS2_PLACEMENT_3D('',#14359,#11343,#11344);
#9718=AXIS2_PLACEMENT_3D('',#14362,#11346,#11347);
#9719=AXIS2_PLACEMENT_3D('',#14363,#11348,#11349);
#9720=AXIS2_PLACEMENT_3D('',#14365,#11350,#11351);
#9721=AXIS2_PLACEMENT_3D('',#14368,#11353,#11354);
#9722=AXIS2_PLACEMENT_3D('',#14369,#11355,#11356);
#9723=AXIS2_PLACEMENT_3D('',#14371,#11357,#11358);
#9724=AXIS2_PLACEMENT_3D('',#14374,#11360,#11361);
#9725=AXIS2_PLACEMENT_3D('',#14375,#11362,#11363);
#9726=AXIS2_PLACEMENT_3D('',#14377,#11364,#11365);
#9727=AXIS2_PLACEMENT_3D('',#14380,#11367,#11368);
#9728=AXIS2_PLACEMENT_3D('',#14381,#11369,#11370);
#9729=AXIS2_PLACEMENT_3D('',#14383,#11371,#11372);
#9730=AXIS2_PLACEMENT_3D('',#14386,#11374,#11375);
#9731=AXIS2_PLACEMENT_3D('',#14387,#11376,#11377);
#9732=AXIS2_PLACEMENT_3D('',#14389,#11378,#11379);
#9733=AXIS2_PLACEMENT_3D('',#14392,#11381,#11382);
#9734=AXIS2_PLACEMENT_3D('',#14393,#11383,#11384);
#9735=AXIS2_PLACEMENT_3D('',#14402,#11389,#11390);
#9736=AXIS2_PLACEMENT_3D('',#14411,#11395,#11396);
#9737=AXIS2_PLACEMENT_3D('',#14417,#11400,#11401);
#9738=AXIS2_PLACEMENT_3D('',#14423,#11405,#11406);
#9739=AXIS2_PLACEMENT_3D('',#14430,#11411,#11412);
#9740=AXIS2_PLACEMENT_3D('',#14434,#11415,#11416);
#9741=AXIS2_PLACEMENT_3D('',#14439,#11420,#11421);
#9742=AXIS2_PLACEMENT_3D('',#14441,#11423,#11424);
#9743=AXIS2_PLACEMENT_3D('',#14442,#11425,#11426);
#9744=AXIS2_PLACEMENT_3D('',#14443,#11427,#11428);
#9745=AXIS2_PLACEMENT_3D('',#14444,#11429,#11430);
#9746=AXIS2_PLACEMENT_3D('',#14446,#11431,#11432);
#9747=AXIS2_PLACEMENT_3D('',#14449,#11434,#11435);
#9748=AXIS2_PLACEMENT_3D('',#14450,#11436,#11437);
#9749=AXIS2_PLACEMENT_3D('',#14452,#11438,#11439);
#9750=AXIS2_PLACEMENT_3D('',#14455,#11441,#11442);
#9751=AXIS2_PLACEMENT_3D('',#14456,#11443,#11444);
#9752=AXIS2_PLACEMENT_3D('',#14457,#11445,#11446);
#9753=AXIS2_PLACEMENT_3D('',#14458,#11447,#11448);
#9754=AXIS2_PLACEMENT_3D('',#14459,#11449,#11450);
#9755=AXIS2_PLACEMENT_3D('',#14461,#11451,#11452);
#9756=AXIS2_PLACEMENT_3D('',#14464,#11454,#11455);
#9757=AXIS2_PLACEMENT_3D('',#14465,#11456,#11457);
#9758=AXIS2_PLACEMENT_3D('',#14467,#11458,#11459);
#9759=AXIS2_PLACEMENT_3D('',#14470,#11461,#11462);
#9760=AXIS2_PLACEMENT_3D('',#14471,#11463,#11464);
#9761=AXIS2_PLACEMENT_3D('',#14472,#11465,#11466);
#9762=AXIS2_PLACEMENT_3D('',#14473,#11467,#11468);
#9763=AXIS2_PLACEMENT_3D('',#14474,#11469,#11470);
#9764=AXIS2_PLACEMENT_3D('',#14476,#11471,#11472);
#9765=AXIS2_PLACEMENT_3D('',#14479,#11474,#11475);
#9766=AXIS2_PLACEMENT_3D('',#14480,#11476,#11477);
#9767=AXIS2_PLACEMENT_3D('',#14482,#11478,#11479);
#9768=AXIS2_PLACEMENT_3D('',#14485,#11481,#11482);
#9769=AXIS2_PLACEMENT_3D('',#14486,#11483,#11484);
#9770=AXIS2_PLACEMENT_3D('',#14487,#11485,#11486);
#9771=AXIS2_PLACEMENT_3D('',#14488,#11487,#11488);
#9772=AXIS2_PLACEMENT_3D('',#14489,#11489,#11490);
#9773=AXIS2_PLACEMENT_3D('',#14491,#11491,#11492);
#9774=AXIS2_PLACEMENT_3D('',#14494,#11494,#11495);
#9775=AXIS2_PLACEMENT_3D('',#14495,#11496,#11497);
#9776=AXIS2_PLACEMENT_3D('',#14497,#11498,#11499);
#9777=AXIS2_PLACEMENT_3D('',#14500,#11501,#11502);
#9778=AXIS2_PLACEMENT_3D('',#14501,#11503,#11504);
#9779=AXIS2_PLACEMENT_3D('',#14502,#11505,#11506);
#9780=AXIS2_PLACEMENT_3D('',#14503,#11507,#11508);
#9781=AXIS2_PLACEMENT_3D('',#14504,#11509,#11510);
#9782=AXIS2_PLACEMENT_3D('',#14506,#11511,#11512);
#9783=AXIS2_PLACEMENT_3D('',#14509,#11514,#11515);
#9784=AXIS2_PLACEMENT_3D('',#14510,#11516,#11517);
#9785=AXIS2_PLACEMENT_3D('',#14512,#11518,#11519);
#9786=AXIS2_PLACEMENT_3D('',#14515,#11521,#11522);
#9787=AXIS2_PLACEMENT_3D('',#14516,#11523,#11524);
#9788=AXIS2_PLACEMENT_3D('',#14517,#11525,#11526);
#9789=AXIS2_PLACEMENT_3D('',#14518,#11527,#11528);
#9790=AXIS2_PLACEMENT_3D('',#14519,#11529,#11530);
#9791=AXIS2_PLACEMENT_3D('',#14524,#11532,#11533);
#9792=AXIS2_PLACEMENT_3D('',#14527,#11535,#11536);
#9793=AXIS2_PLACEMENT_3D('',#14528,#11537,#11538);
#9794=AXIS2_PLACEMENT_3D('',#14533,#11540,#11541);
#9795=AXIS2_PLACEMENT_3D('',#14536,#11543,#11544);
#9796=AXIS2_PLACEMENT_3D('',#14537,#11545,#11546);
#9797=AXIS2_PLACEMENT_3D('',#14542,#11548,#11549);
#9798=AXIS2_PLACEMENT_3D('',#14545,#11551,#11552);
#9799=AXIS2_PLACEMENT_3D('',#14546,#11553,#11554);
#9800=AXIS2_PLACEMENT_3D('',#14551,#11556,#11557);
#9801=AXIS2_PLACEMENT_3D('',#14554,#11559,#11560);
#9802=AXIS2_PLACEMENT_3D('',#14555,#11561,#11562);
#9803=AXIS2_PLACEMENT_3D('',#14556,#11563,#11564);
#9804=AXIS2_PLACEMENT_3D('',#14557,#11565,#11566);
#9805=AXIS2_PLACEMENT_3D('',#14558,#11567,#11568);
#9806=AXIS2_PLACEMENT_3D('',#14559,#11569,#11570);
#9807=AXIS2_PLACEMENT_3D('',#14561,#11571,#11572);
#9808=AXIS2_PLACEMENT_3D('',#14562,#11573,#11574);
#9809=AXIS2_PLACEMENT_3D('',#14563,#11575,#11576);
#9810=AXIS2_PLACEMENT_3D('',#14564,#11577,#11578);
#9811=AXIS2_PLACEMENT_3D('',#14565,#11579,#11580);
#9812=AXIS2_PLACEMENT_3D('',#14566,#11581,#11582);
#9813=AXIS2_PLACEMENT_3D('',#14567,#11583,#11584);
#9814=AXIS2_PLACEMENT_3D('',#14568,#11585,#11586);
#9815=AXIS2_PLACEMENT_3D('',#14569,#11587,#11588);
#9816=AXIS2_PLACEMENT_3D('',#14570,#11589,#11590);
#9817=AXIS2_PLACEMENT_3D('',#14572,#11591,#11592);
#9818=AXIS2_PLACEMENT_3D('',#14575,#11594,#11595);
#9819=AXIS2_PLACEMENT_3D('',#14576,#11596,#11597);
#9820=AXIS2_PLACEMENT_3D('',#14578,#11598,#11599);
#9821=AXIS2_PLACEMENT_3D('',#14579,#11600,#11601);
#9822=AXIS2_PLACEMENT_3D('',#14581,#11603,#11604);
#9823=AXIS2_PLACEMENT_3D('',#14582,#11605,#11606);
#9824=AXIS2_PLACEMENT_3D('',#14583,#11607,#11608);
#9825=AXIS2_PLACEMENT_3D('',#14588,#11610,#11611);
#9826=AXIS2_PLACEMENT_3D('',#14591,#11613,#11614);
#9827=AXIS2_PLACEMENT_3D('',#14592,#11615,#11616);
#9828=AXIS2_PLACEMENT_3D('',#14597,#11618,#11619);
#9829=AXIS2_PLACEMENT_3D('',#14600,#11621,#11622);
#9830=AXIS2_PLACEMENT_3D('',#14601,#11623,#11624);
#9831=AXIS2_PLACEMENT_3D('',#14606,#11626,#11627);
#9832=AXIS2_PLACEMENT_3D('',#14609,#11629,#11630);
#9833=AXIS2_PLACEMENT_3D('',#14610,#11631,#11632);
#9834=AXIS2_PLACEMENT_3D('',#14615,#11634,#11635);
#9835=AXIS2_PLACEMENT_3D('',#14618,#11637,#11638);
#9836=AXIS2_PLACEMENT_3D('',#14619,#11639,#11640);
#9837=AXIS2_PLACEMENT_3D('',#14620,#11641,#11642);
#9838=AXIS2_PLACEMENT_3D('',#14621,#11643,#11644);
#9839=AXIS2_PLACEMENT_3D('',#14622,#11645,#11646);
#9840=AXIS2_PLACEMENT_3D('',#14623,#11647,#11648);
#9841=AXIS2_PLACEMENT_3D('',#14625,#11649,#11650);
#9842=AXIS2_PLACEMENT_3D('',#14626,#11651,#11652);
#9843=AXIS2_PLACEMENT_3D('',#14627,#11653,#11654);
#9844=AXIS2_PLACEMENT_3D('',#14628,#11655,#11656);
#9845=AXIS2_PLACEMENT_3D('',#14629,#11657,#11658);
#9846=AXIS2_PLACEMENT_3D('',#14630,#11659,#11660);
#9847=AXIS2_PLACEMENT_3D('',#14631,#11661,#11662);
#9848=AXIS2_PLACEMENT_3D('',#14632,#11663,#11664);
#9849=AXIS2_PLACEMENT_3D('',#14633,#11665,#11666);
#9850=AXIS2_PLACEMENT_3D('',#14634,#11667,#11668);
#9851=AXIS2_PLACEMENT_3D('',#14637,#11670,#11671);
#9852=AXIS2_PLACEMENT_3D('',#14638,#11672,#11673);
#9853=AXIS2_PLACEMENT_3D('',#14640,#11674,#11675);
#9854=AXIS2_PLACEMENT_3D('',#14641,#11676,#11677);
#9855=AXIS2_PLACEMENT_3D('',#14643,#11678,#11679);
#9856=AXIS2_PLACEMENT_3D('',#14645,#11681,#11682);
#9857=AXIS2_PLACEMENT_3D('',#14646,#11683,#11684);
#9858=AXIS2_PLACEMENT_3D('',#14647,#11685,#11686);
#9859=AXIS2_PLACEMENT_3D('',#14656,#11691,#11692);
#9860=AXIS2_PLACEMENT_3D('',#14665,#11697,#11698);
#9861=AXIS2_PLACEMENT_3D('',#14670,#11700,#11701);
#9862=AXIS2_PLACEMENT_3D('',#14673,#11703,#11704);
#9863=AXIS2_PLACEMENT_3D('',#14674,#11705,#11706);
#9864=AXIS2_PLACEMENT_3D('',#14675,#11707,#11708);
#9865=AXIS2_PLACEMENT_3D('',#14676,#11709,#11710);
#9866=AXIS2_PLACEMENT_3D('',#14677,#11711,#11712);
#9867=AXIS2_PLACEMENT_3D('',#14678,#11713,#11714);
#9868=AXIS2_PLACEMENT_3D('',#14679,#11715,#11716);
#9869=AXIS2_PLACEMENT_3D('',#14680,#11717,#11718);
#9870=AXIS2_PLACEMENT_3D('',#14684,#11720,#11721);
#9871=AXIS2_PLACEMENT_3D('',#14686,#11723,#11724);
#9872=AXIS2_PLACEMENT_3D('',#14690,#11727,#11728);
#9873=AXIS2_PLACEMENT_3D('',#14694,#11731,#11732);
#9874=AXIS2_PLACEMENT_3D('',#14695,#11733,#11734);
#9875=AXIS2_PLACEMENT_3D('',#14696,#11735,#11736);
#9876=AXIS2_PLACEMENT_3D('',#14697,#11737,#11738);
#9877=AXIS2_PLACEMENT_3D('',#14698,#11739,#11740);
#9878=AXIS2_PLACEMENT_3D('',#14699,#11741,#11742);
#9879=AXIS2_PLACEMENT_3D('',#14702,#11743,#11744);
#9880=AXIS2_PLACEMENT_3D('',#14703,#11745,#11746);
#9881=AXIS2_PLACEMENT_3D('',#14705,#11747,#11748);
#9882=AXIS2_PLACEMENT_3D('',#14707,#11749,#11750);
#9883=AXIS2_PLACEMENT_3D('',#14708,#11751,#11752);
#9884=AXIS2_PLACEMENT_3D('',#14709,#11753,#11754);
#9885=AXIS2_PLACEMENT_3D('',#14712,#11756,#11757);
#9886=AXIS2_PLACEMENT_3D('',#14713,#11758,#11759);
#9887=AXIS2_PLACEMENT_3D('',#14715,#11760,#11761);
#9888=AXIS2_PLACEMENT_3D('',#14718,#11763,#11764);
#9889=AXIS2_PLACEMENT_3D('',#14719,#11765,#11766);
#9890=AXIS2_PLACEMENT_3D('',#14722,#11768,#11769);
#9891=AXIS2_PLACEMENT_3D('',#14723,#11770,#11771);
#9892=AXIS2_PLACEMENT_3D('',#14724,#11772,#11773);
#9893=AXIS2_PLACEMENT_3D('',#14726,#11774,#11775);
#9894=AXIS2_PLACEMENT_3D('',#14728,#11777,#11778);
#9895=AXIS2_PLACEMENT_3D('',#14730,#11779,#11780);
#9896=AXIS2_PLACEMENT_3D('',#14731,#11781,#11782);
#9897=AXIS2_PLACEMENT_3D('',#14733,#11784,#11785);
#9898=AXIS2_PLACEMENT_3D('',#14734,#11786,#11787);
#9899=AXIS2_PLACEMENT_3D('',#14737,#11788,#11789);
#9900=AXIS2_PLACEMENT_3D('',#14738,#11790,#11791);
#9901=AXIS2_PLACEMENT_3D('',#14740,#11792,#11793);
#9902=AXIS2_PLACEMENT_3D('',#14742,#11794,#11795);
#9903=AXIS2_PLACEMENT_3D('',#14743,#11796,#11797);
#9904=AXIS2_PLACEMENT_3D('',#14744,#11798,#11799);
#9905=AXIS2_PLACEMENT_3D('',#14746,#11800,#11801);
#9906=AXIS2_PLACEMENT_3D('',#14748,#11803,#11804);
#9907=AXIS2_PLACEMENT_3D('',#14750,#11805,#11806);
#9908=AXIS2_PLACEMENT_3D('',#14752,#11807,#11808);
#9909=AXIS2_PLACEMENT_3D('',#14753,#11809,#11810);
#9910=AXIS2_PLACEMENT_3D('',#14755,#11811,#11812);
#9911=AXIS2_PLACEMENT_3D('',#14757,#11814,#11815);
#9912=AXIS2_PLACEMENT_3D('',#14759,#11816,#11817);
#9913=AXIS2_PLACEMENT_3D('',#14761,#11819,#11820);
#9914=AXIS2_PLACEMENT_3D('',#14763,#11821,#11822);
#9915=AXIS2_PLACEMENT_3D('',#14765,#11824,#11825);
#9916=AXIS2_PLACEMENT_3D('',#14766,#11826,#11827);
#9917=AXIS2_PLACEMENT_3D('',#14768,#11829,#11830);
#9918=AXIS2_PLACEMENT_3D('',#14769,#11831,#11832);
#9919=AXIS2_PLACEMENT_3D('',#14772,#11833,#11834);
#9920=AXIS2_PLACEMENT_3D('',#14773,#11835,#11836);
#9921=AXIS2_PLACEMENT_3D('',#14776,#11837,#11838);
#9922=AXIS2_PLACEMENT_3D('',#14777,#11839,#11840);
#9923=AXIS2_PLACEMENT_3D('',#14780,#11841,#11842);
#9924=AXIS2_PLACEMENT_3D('',#14781,#11843,#11844);
#9925=AXIS2_PLACEMENT_3D('',#14784,#11845,#11846);
#9926=AXIS2_PLACEMENT_3D('',#14785,#11847,#11848);
#9927=AXIS2_PLACEMENT_3D('',#14788,#11849,#11850);
#9928=AXIS2_PLACEMENT_3D('',#14789,#11851,#11852);
#9929=AXIS2_PLACEMENT_3D('',#14792,#11853,#11854);
#9930=AXIS2_PLACEMENT_3D('',#14793,#11855,#11856);
#9931=AXIS2_PLACEMENT_3D('',#14796,#11857,#11858);
#9932=AXIS2_PLACEMENT_3D('',#14797,#11859,#11860);
#9933=AXIS2_PLACEMENT_3D('',#14800,#11861,#11862);
#9934=AXIS2_PLACEMENT_3D('',#14801,#11863,#11864);
#9935=AXIS2_PLACEMENT_3D('',#14802,#11865,#11866);
#9936=AXIS2_PLACEMENT_3D('',#14828,#11867,#11868);
#9937=AXIS2_PLACEMENT_3D('',#14852,#11869,#11870);
#9938=AXIS2_PLACEMENT_3D('',#14853,#11871,#11872);
#9939=AXIS2_PLACEMENT_3D('',#14855,#11873,#11874);
#9940=AXIS2_PLACEMENT_3D('',#14880,#11875,#11876);
#9941=AXIS2_PLACEMENT_3D('',#14905,#11877,#11878);
#9942=AXIS2_PLACEMENT_3D('',#14921,#11880,#11881);
#9943=AXIS2_PLACEMENT_3D('',#14936,#11882,#11883);
#9944=AXIS2_PLACEMENT_3D('',#14961,#11884,#11885);
#9945=AXIS2_PLACEMENT_3D('',#14986,#11886,#11887);
#9946=AXIS2_PLACEMENT_3D('',#15011,#11888,#11889);
#9947=AXIS2_PLACEMENT_3D('',#15035,#11890,#11891);
#9948=AXIS2_PLACEMENT_3D('',#15036,#11892,#11893);
#9949=AXIS2_PLACEMENT_3D('',#15038,#11894,#11895);
#9950=AXIS2_PLACEMENT_3D('',#15039,#11896,#11897);
#9951=AXIS2_PLACEMENT_3D('',#15040,#11898,#11899);
#9952=AXIS2_PLACEMENT_3D('',#15064,#11900,#11901);
#9953=AXIS2_PLACEMENT_3D('',#15065,#11902,#11903);
#9954=AXIS2_PLACEMENT_3D('',#15067,#11904,#11905);
#9955=AXIS2_PLACEMENT_3D('',#15068,#11906,#11907);
#9956=AXIS2_PLACEMENT_3D('',#15069,#11908,#11909);
#9957=AXIS2_PLACEMENT_3D('',#15093,#11910,#11911);
#9958=AXIS2_PLACEMENT_3D('',#15094,#11912,#11913);
#9959=AXIS2_PLACEMENT_3D('',#15096,#11914,#11915);
#9960=AXIS2_PLACEMENT_3D('',#15097,#11916,#11917);
#9961=AXIS2_PLACEMENT_3D('',#15098,#11918,#11919);
#9962=AXIS2_PLACEMENT_3D('',#15113,#11920,#11921);
#9963=AXIS2_PLACEMENT_3D('',#15126,#11922,#11923);
#9964=AXIS2_PLACEMENT_3D('',#15128,#11924,#11925);
#9965=AXIS2_PLACEMENT_3D('',#15129,#11926,#11927);
#9966=AXIS2_PLACEMENT_3D('',#15130,#11928,#11929);
#9967=AXIS2_PLACEMENT_3D('',#15154,#11930,#11931);
#9968=AXIS2_PLACEMENT_3D('',#15155,#11932,#11933);
#9969=AXIS2_PLACEMENT_3D('',#15157,#11934,#11935);
#9970=AXIS2_PLACEMENT_3D('',#15158,#11936,#11937);
#9971=AXIS2_PLACEMENT_3D('',#15159,#11938,#11939);
#9972=AXIS2_PLACEMENT_3D('',#15183,#11940,#11941);
#9973=AXIS2_PLACEMENT_3D('',#15184,#11942,#11943);
#9974=AXIS2_PLACEMENT_3D('',#15186,#11944,#11945);
#9975=AXIS2_PLACEMENT_3D('',#15187,#11946,#11947);
#9976=AXIS2_PLACEMENT_3D('',#15188,#11948,#11949);
#9977=AXIS2_PLACEMENT_3D('',#15212,#11950,#11951);
#9978=AXIS2_PLACEMENT_3D('',#15213,#11952,#11953);
#9979=AXIS2_PLACEMENT_3D('',#15215,#11954,#11955);
#9980=AXIS2_PLACEMENT_3D('',#15218,#11957,#11958);
#9981=AXIS2_PLACEMENT_3D('',#15242,#11959,#11960);
#9982=AXIS2_PLACEMENT_3D('',#15243,#11961,#11962);
#9983=AXIS2_PLACEMENT_3D('',#15244,#11963,#11964);
#9984=AXIS2_PLACEMENT_3D('',#15245,#11965,#11966);
#9985=AXIS2_PLACEMENT_3D('',#15246,#11967,#11968);
#9986=AXIS2_PLACEMENT_3D('',#15247,#11969,#11970);
#9987=AXIS2_PLACEMENT_3D('',#15248,#11971,#11972);
#9988=AXIS2_PLACEMENT_3D('',#15249,#11973,#11974);
#9989=AXIS2_PLACEMENT_3D('',#15250,#11975,#11976);
#9990=AXIS2_PLACEMENT_3D('',#15252,#11977,#11978);
#9991=AXIS2_PLACEMENT_3D('',#15254,#11979,#11980);
#9992=AXIS2_PLACEMENT_3D('',#15255,#11981,#11982);
#9993=AXIS2_PLACEMENT_3D('',#15257,#11983,#11984);
#9994=AXIS2_PLACEMENT_3D('',#15259,#11986,#11987);
#9995=AXIS2_PLACEMENT_3D('',#15261,#11988,#11989);
#9996=AXIS2_PLACEMENT_3D('',#15262,#11990,#11991);
#9997=AXIS2_PLACEMENT_3D('',#15264,#11993,#11994);
#9998=AXIS2_PLACEMENT_3D('',#15266,#11995,#11996);
#9999=AXIS2_PLACEMENT_3D('',#15268,#11997,#11998);
#10000=AXIS2_PLACEMENT_3D('',#15269,#11999,#12000);
#10001=AXIS2_PLACEMENT_3D('',#15271,#12001,#12002);
#10002=AXIS2_PLACEMENT_3D('',#15273,#12004,#12005);
#10003=AXIS2_PLACEMENT_3D('',#15275,#12006,#12007);
#10004=AXIS2_PLACEMENT_3D('',#15276,#12008,#12009);
#10005=AXIS2_PLACEMENT_3D('',#15278,#12011,#12012);
#10006=AXIS2_PLACEMENT_3D('',#15279,#12013,#12014);
#10007=AXIS2_PLACEMENT_3D('',#15280,#12015,#12016);
#10008=AXIS2_PLACEMENT_3D('',#15281,#12017,#12018);
#10009=AXIS2_PLACEMENT_3D('',#15282,#12019,#12020);
#10010=AXIS2_PLACEMENT_3D('',#15283,#12021,#12022);
#10011=AXIS2_PLACEMENT_3D('',#15284,#12023,#12024);
#10012=AXIS2_PLACEMENT_3D('',#15293,#12029,#12030);
#10013=AXIS2_PLACEMENT_3D('',#15299,#12034,#12035);
#10014=AXIS2_PLACEMENT_3D('',#15305,#12039,#12040);
#10015=AXIS2_PLACEMENT_3D('',#15311,#12044,#12045);
#10016=AXIS2_PLACEMENT_3D('',#15317,#12049,#12050);
#10017=AXIS2_PLACEMENT_3D('',#15320,#12053,#12054);
#10018=AXIS2_PLACEMENT_3D('',#15321,#12055,#12056);
#10019=AXIS2_PLACEMENT_3D('',#15322,#12057,#12058);
#10020=AXIS2_PLACEMENT_3D('',#15324,#12059,#12060);
#10021=AXIS2_PLACEMENT_3D('',#15326,#12061,#12062);
#10022=AXIS2_PLACEMENT_3D('',#15327,#12063,#12064);
#10023=AXIS2_PLACEMENT_3D('',#15330,#12066,#12067);
#10024=AXIS2_PLACEMENT_3D('',#15331,#12068,#12069);
#10025=AXIS2_PLACEMENT_3D('',#15332,#12070,#12071);
#10026=AXIS2_PLACEMENT_3D('',#15334,#12072,#12073);
#10027=AXIS2_PLACEMENT_3D('',#15335,#12074,#12075);
#10028=AXIS2_PLACEMENT_3D('',#15337,#12076,#12077);
#10029=AXIS2_PLACEMENT_3D('',#15339,#12079,#12080);
#10030=AXIS2_PLACEMENT_3D('',#15341,#12081,#12082);
#10031=AXIS2_PLACEMENT_3D('',#15343,#12084,#12085);
#10032=AXIS2_PLACEMENT_3D('',#15345,#12086,#12087);
#10033=AXIS2_PLACEMENT_3D('',#15347,#12089,#12090);
#10034=AXIS2_PLACEMENT_3D('',#15349,#12091,#12092);
#10035=AXIS2_PLACEMENT_3D('',#15350,#12093,#12094);
#10036=AXIS2_PLACEMENT_3D('',#15352,#12095,#12096);
#10037=AXIS2_PLACEMENT_3D('',#15354,#12098,#12099);
#10038=AXIS2_PLACEMENT_3D('',#15356,#12100,#12101);
#10039=AXIS2_PLACEMENT_3D('',#15358,#12103,#12104);
#10040=AXIS2_PLACEMENT_3D('',#15360,#12106,#12107);
#10041=AXIS2_PLACEMENT_3D('',#15361,#12108,#12109);
#10042=AXIS2_PLACEMENT_3D('',#15362,#12110,#12111);
#10043=AXIS2_PLACEMENT_3D('',#15365,#12112,#12113);
#10044=AXIS2_PLACEMENT_3D('',#15366,#12114,#12115);
#10045=AXIS2_PLACEMENT_3D('',#15368,#12116,#12117);
#10046=AXIS2_PLACEMENT_3D('',#15370,#12118,#12119);
#10047=AXIS2_PLACEMENT_3D('',#15371,#12120,#12121);
#10048=AXIS2_PLACEMENT_3D('',#15372,#12122,#12123);
#10049=AXIS2_PLACEMENT_3D('',#15375,#12125,#12126);
#10050=AXIS2_PLACEMENT_3D('',#15376,#12127,#12128);
#10051=AXIS2_PLACEMENT_3D('',#15378,#12129,#12130);
#10052=AXIS2_PLACEMENT_3D('',#15381,#12132,#12133);
#10053=AXIS2_PLACEMENT_3D('',#15382,#12134,#12135);
#10054=AXIS2_PLACEMENT_3D('',#15385,#12137,#12138);
#10055=AXIS2_PLACEMENT_3D('',#15386,#12139,#12140);
#10056=AXIS2_PLACEMENT_3D('',#15387,#12141,#12142);
#10057=AXIS2_PLACEMENT_3D('',#15389,#12143,#12144);
#10058=AXIS2_PLACEMENT_3D('',#15391,#12146,#12147);
#10059=AXIS2_PLACEMENT_3D('',#15393,#12148,#12149);
#10060=AXIS2_PLACEMENT_3D('',#15394,#12150,#12151);
#10061=AXIS2_PLACEMENT_3D('',#15396,#12153,#12154);
#10062=AXIS2_PLACEMENT_3D('',#15397,#12155,#12156);
#10063=AXIS2_PLACEMENT_3D('',#15400,#12157,#12158);
#10064=AXIS2_PLACEMENT_3D('',#15401,#12159,#12160);
#10065=AXIS2_PLACEMENT_3D('',#15403,#12161,#12162);
#10066=AXIS2_PLACEMENT_3D('',#15405,#12163,#12164);
#10067=AXIS2_PLACEMENT_3D('',#15406,#12165,#12166);
#10068=AXIS2_PLACEMENT_3D('',#15407,#12167,#12168);
#10069=AXIS2_PLACEMENT_3D('',#15409,#12169,#12170);
#10070=AXIS2_PLACEMENT_3D('',#15411,#12172,#12173);
#10071=AXIS2_PLACEMENT_3D('',#15413,#12174,#12175);
#10072=AXIS2_PLACEMENT_3D('',#15415,#12176,#12177);
#10073=AXIS2_PLACEMENT_3D('',#15416,#12178,#12179);
#10074=AXIS2_PLACEMENT_3D('',#15418,#12180,#12181);
#10075=AXIS2_PLACEMENT_3D('',#15420,#12183,#12184);
#10076=AXIS2_PLACEMENT_3D('',#15422,#12185,#12186);
#10077=AXIS2_PLACEMENT_3D('',#15424,#12188,#12189);
#10078=AXIS2_PLACEMENT_3D('',#15426,#12190,#12191);
#10079=AXIS2_PLACEMENT_3D('',#15428,#12193,#12194);
#10080=AXIS2_PLACEMENT_3D('',#15429,#12195,#12196);
#10081=AXIS2_PLACEMENT_3D('',#15431,#12198,#12199);
#10082=AXIS2_PLACEMENT_3D('',#15432,#12200,#12201);
#10083=AXIS2_PLACEMENT_3D('',#15435,#12202,#12203);
#10084=AXIS2_PLACEMENT_3D('',#15436,#12204,#12205);
#10085=AXIS2_PLACEMENT_3D('',#15439,#12206,#12207);
#10086=AXIS2_PLACEMENT_3D('',#15440,#12208,#12209);
#10087=AXIS2_PLACEMENT_3D('',#15443,#12210,#12211);
#10088=AXIS2_PLACEMENT_3D('',#15444,#12212,#12213);
#10089=AXIS2_PLACEMENT_3D('',#15447,#12214,#12215);
#10090=AXIS2_PLACEMENT_3D('',#15448,#12216,#12217);
#10091=AXIS2_PLACEMENT_3D('',#15451,#12218,#12219);
#10092=AXIS2_PLACEMENT_3D('',#15452,#12220,#12221);
#10093=AXIS2_PLACEMENT_3D('',#15455,#12222,#12223);
#10094=AXIS2_PLACEMENT_3D('',#15456,#12224,#12225);
#10095=AXIS2_PLACEMENT_3D('',#15459,#12226,#12227);
#10096=AXIS2_PLACEMENT_3D('',#15460,#12228,#12229);
#10097=AXIS2_PLACEMENT_3D('',#15461,#12230,#12231);
#10098=AXIS2_PLACEMENT_3D('',#15487,#12232,#12233);
#10099=AXIS2_PLACEMENT_3D('',#15511,#12234,#12235);
#10100=AXIS2_PLACEMENT_3D('',#15512,#12236,#12237);
#10101=AXIS2_PLACEMENT_3D('',#15514,#12238,#12239);
#10102=AXIS2_PLACEMENT_3D('',#15539,#12240,#12241);
#10103=AXIS2_PLACEMENT_3D('',#15564,#12242,#12243);
#10104=AXIS2_PLACEMENT_3D('',#15567,#12245,#12246);
#10105=AXIS2_PLACEMENT_3D('',#15569,#12247,#12248);
#10106=AXIS2_PLACEMENT_3D('',#15594,#12249,#12250);
#10107=AXIS2_PLACEMENT_3D('',#15619,#12251,#12252);
#10108=AXIS2_PLACEMENT_3D('',#15644,#12253,#12254);
#10109=AXIS2_PLACEMENT_3D('',#15668,#12255,#12256);
#10110=AXIS2_PLACEMENT_3D('',#15669,#12257,#12258);
#10111=AXIS2_PLACEMENT_3D('',#15671,#12259,#12260);
#10112=AXIS2_PLACEMENT_3D('',#15672,#12261,#12262);
#10113=AXIS2_PLACEMENT_3D('',#15673,#12263,#12264);
#10114=AXIS2_PLACEMENT_3D('',#15697,#12265,#12266);
#10115=AXIS2_PLACEMENT_3D('',#15698,#12267,#12268);
#10116=AXIS2_PLACEMENT_3D('',#15700,#12269,#12270);
#10117=AXIS2_PLACEMENT_3D('',#15701,#12271,#12272);
#10118=AXIS2_PLACEMENT_3D('',#15702,#12273,#12274);
#10119=AXIS2_PLACEMENT_3D('',#15726,#12275,#12276);
#10120=AXIS2_PLACEMENT_3D('',#15727,#12277,#12278);
#10121=AXIS2_PLACEMENT_3D('',#15729,#12279,#12280);
#10122=AXIS2_PLACEMENT_3D('',#15731,#12281,#12282);
#10123=AXIS2_PLACEMENT_3D('',#15732,#12283,#12284);
#10124=AXIS2_PLACEMENT_3D('',#15733,#12285,#12286);
#10125=AXIS2_PLACEMENT_3D('',#15757,#12287,#12288);
#10126=AXIS2_PLACEMENT_3D('',#15758,#12289,#12290);
#10127=AXIS2_PLACEMENT_3D('',#15760,#12291,#12292);
#10128=AXIS2_PLACEMENT_3D('',#15761,#12293,#12294);
#10129=AXIS2_PLACEMENT_3D('',#15762,#12295,#12296);
#10130=AXIS2_PLACEMENT_3D('',#15786,#12297,#12298);
#10131=AXIS2_PLACEMENT_3D('',#15787,#12299,#12300);
#10132=AXIS2_PLACEMENT_3D('',#15789,#12301,#12302);
#10133=AXIS2_PLACEMENT_3D('',#15790,#12303,#12304);
#10134=AXIS2_PLACEMENT_3D('',#15791,#12305,#12306);
#10135=AXIS2_PLACEMENT_3D('',#15815,#12307,#12308);
#10136=AXIS2_PLACEMENT_3D('',#15816,#12309,#12310);
#10137=AXIS2_PLACEMENT_3D('',#15818,#12311,#12312);
#10138=AXIS2_PLACEMENT_3D('',#15821,#12314,#12315);
#10139=AXIS2_PLACEMENT_3D('',#15845,#12316,#12317);
#10140=AXIS2_PLACEMENT_3D('',#15846,#12318,#12319);
#10141=AXIS2_PLACEMENT_3D('',#15847,#12320,#12321);
#10142=AXIS2_PLACEMENT_3D('',#15848,#12322,#12323);
#10143=AXIS2_PLACEMENT_3D('',#15849,#12324,#12325);
#10144=AXIS2_PLACEMENT_3D('',#15850,#12326,#12327);
#10145=AXIS2_PLACEMENT_3D('',#15851,#12328,#12329);
#10146=AXIS2_PLACEMENT_3D('',#15852,#12330,#12331);
#10147=AXIS2_PLACEMENT_3D('',#15853,#12332,#12333);
#10148=AXIS2_PLACEMENT_3D('',#15855,#12334,#12335);
#10149=AXIS2_PLACEMENT_3D('',#15857,#12336,#12337);
#10150=AXIS2_PLACEMENT_3D('',#15858,#12338,#12339);
#10151=AXIS2_PLACEMENT_3D('',#15860,#12340,#12341);
#10152=AXIS2_PLACEMENT_3D('',#15862,#12343,#12344);
#10153=AXIS2_PLACEMENT_3D('',#15864,#12345,#12346);
#10154=AXIS2_PLACEMENT_3D('',#15865,#12347,#12348);
#10155=AXIS2_PLACEMENT_3D('',#15867,#12350,#12351);
#10156=AXIS2_PLACEMENT_3D('',#15869,#12352,#12353);
#10157=AXIS2_PLACEMENT_3D('',#15871,#12354,#12355);
#10158=AXIS2_PLACEMENT_3D('',#15872,#12356,#12357);
#10159=AXIS2_PLACEMENT_3D('',#15874,#12358,#12359);
#10160=AXIS2_PLACEMENT_3D('',#15876,#12361,#12362);
#10161=AXIS2_PLACEMENT_3D('',#15878,#12363,#12364);
#10162=AXIS2_PLACEMENT_3D('',#15879,#12365,#12366);
#10163=AXIS2_PLACEMENT_3D('',#15881,#12368,#12369);
#10164=AXIS2_PLACEMENT_3D('',#15882,#12370,#12371);
#10165=AXIS2_PLACEMENT_3D('',#15883,#12372,#12373);
#10166=AXIS2_PLACEMENT_3D('',#15884,#12374,#12375);
#10167=AXIS2_PLACEMENT_3D('',#15885,#12376,#12377);
#10168=AXIS2_PLACEMENT_3D('',#15886,#12378,#12379);
#10169=AXIS2_PLACEMENT_3D('',#15887,#12380,#12381);
#10170=AXIS2_PLACEMENT_3D('',#15896,#12386,#12387);
#10171=AXIS2_PLACEMENT_3D('',#15902,#12391,#12392);
#10172=AXIS2_PLACEMENT_3D('',#15908,#12396,#12397);
#10173=AXIS2_PLACEMENT_3D('',#15914,#12401,#12402);
#10174=AXIS2_PLACEMENT_3D('',#15920,#12406,#12407);
#10175=AXIS2_PLACEMENT_3D('',#15923,#12410,#12411);
#10176=AXIS2_PLACEMENT_3D('',#15924,#12412,#12413);
#10177=AXIS2_PLACEMENT_3D('',#15925,#12414,#12415);
#10178=AXIS2_PLACEMENT_3D('',#15927,#12416,#12417);
#10179=AXIS2_PLACEMENT_3D('',#15928,#12418,#12419);
#10180=AXIS2_PLACEMENT_3D('',#15930,#12420,#12421);
#10181=AXIS2_PLACEMENT_3D('',#15931,#12422,#12423);
#10182=AXIS2_PLACEMENT_3D('',#15933,#12424,#12425);
#10183=AXIS2_PLACEMENT_3D('',#15935,#12427,#12428);
#10184=AXIS2_PLACEMENT_3D('',#15937,#12429,#12430);
#10185=AXIS2_PLACEMENT_3D('',#15939,#12432,#12433);
#10186=AXIS2_PLACEMENT_3D('',#15941,#12434,#12435);
#10187=AXIS2_PLACEMENT_3D('',#15943,#12437,#12438);
#10188=AXIS2_PLACEMENT_3D('',#15945,#12439,#12440);
#10189=AXIS2_PLACEMENT_3D('',#15946,#12441,#12442);
#10190=AXIS2_PLACEMENT_3D('',#15948,#12443,#12444);
#10191=AXIS2_PLACEMENT_3D('',#15950,#12446,#12447);
#10192=AXIS2_PLACEMENT_3D('',#15952,#12449,#12450);
#10193=AXIS2_PLACEMENT_3D('',#15953,#12451,#12452);
#10194=AXIS2_PLACEMENT_3D('',#15954,#12453,#12454);
#10195=AXIS2_PLACEMENT_3D('',#15956,#12455,#12456);
#10196=AXIS2_PLACEMENT_3D('',#15959,#12458,#12459);
#10197=AXIS2_PLACEMENT_3D('',#15960,#12460,#12461);
#10198=AXIS2_PLACEMENT_3D('',#15961,#12462,#12463);
#10199=AXIS2_PLACEMENT_3D('',#15963,#12464,#12465);
#10200=AXIS2_PLACEMENT_3D('',#15965,#12466,#12467);
#10201=AXIS2_PLACEMENT_3D('',#15966,#12468,#12469);
#10202=AXIS2_PLACEMENT_3D('',#15968,#12470,#12471);
#10203=AXIS2_PLACEMENT_3D('',#15970,#12472,#12473);
#10204=AXIS2_PLACEMENT_3D('',#15971,#12474,#12475);
#10205=AXIS2_PLACEMENT_3D('',#15973,#12477,#12478);
#10206=AXIS2_PLACEMENT_3D('',#15976,#12480,#12481);
#10207=AXIS2_PLACEMENT_3D('',#15977,#12482,#12483);
#10208=AXIS2_PLACEMENT_3D('',#15979,#12484,#12485);
#10209=AXIS2_PLACEMENT_3D('',#15982,#12487,#12488);
#10210=AXIS2_PLACEMENT_3D('',#15983,#12489,#12490);
#10211=AXIS2_PLACEMENT_3D('',#15984,#12491,#12492);
#10212=AXIS2_PLACEMENT_3D('',#15986,#12493,#12494);
#10213=AXIS2_PLACEMENT_3D('',#15988,#12496,#12497);
#10214=AXIS2_PLACEMENT_3D('',#15989,#12498,#12499);
#10215=AXIS2_PLACEMENT_3D('',#15990,#12500,#12501);
#10216=AXIS2_PLACEMENT_3D('',#15991,#12502,#12503);
#10217=AXIS2_PLACEMENT_3D('',#15993,#12504,#12505);
#10218=AXIS2_PLACEMENT_3D('',#15996,#12507,#12508);
#10219=AXIS2_PLACEMENT_3D('',#15997,#12509,#12510);
#10220=AXIS2_PLACEMENT_3D('',#15999,#12511,#12512);
#10221=AXIS2_PLACEMENT_3D('',#16000,#12513,#12514);
#10222=AXIS2_PLACEMENT_3D('',#16003,#12516,#12517);
#10223=AXIS2_PLACEMENT_3D('',#16004,#12518,#12519);
#10224=AXIS2_PLACEMENT_3D('',#16006,#12520,#12521);
#10225=AXIS2_PLACEMENT_3D('',#16009,#12523,#12524);
#10226=AXIS2_PLACEMENT_3D('',#16010,#12525,#12526);
#10227=AXIS2_PLACEMENT_3D('',#16011,#12527,#12528);
#10228=AXIS2_PLACEMENT_3D('',#16012,#12529,#12530);
#10229=AXIS2_PLACEMENT_3D('',#16013,#12531,#12532);
#10230=AXIS2_PLACEMENT_3D('',#16015,#12533,#12534);
#10231=AXIS2_PLACEMENT_3D('',#16018,#12536,#12537);
#10232=AXIS2_PLACEMENT_3D('',#16019,#12538,#12539);
#10233=AXIS2_PLACEMENT_3D('',#16021,#12540,#12541);
#10234=AXIS2_PLACEMENT_3D('',#16024,#12543,#12544);
#10235=AXIS2_PLACEMENT_3D('',#16025,#12545,#12546);
#10236=AXIS2_PLACEMENT_3D('',#16026,#12547,#12548);
#10237=AXIS2_PLACEMENT_3D('',#16027,#12549,#12550);
#10238=AXIS2_PLACEMENT_3D('',#16028,#12551,#12552);
#10239=AXIS2_PLACEMENT_3D('',#16030,#12553,#12554);
#10240=AXIS2_PLACEMENT_3D('',#16033,#12556,#12557);
#10241=AXIS2_PLACEMENT_3D('',#16034,#12558,#12559);
#10242=AXIS2_PLACEMENT_3D('',#16035,#12560,#12561);
#10243=AXIS2_PLACEMENT_3D('',#16036,#12562,#12563);
#10244=AXIS2_PLACEMENT_3D('',#16037,#12564,#12565);
#10245=AXIS2_PLACEMENT_3D('',#16039,#12566,#12567);
#10246=AXIS2_PLACEMENT_3D('',#16042,#12569,#12570);
#10247=AXIS2_PLACEMENT_3D('',#16043,#12571,#12572);
#10248=AXIS2_PLACEMENT_3D('',#16044,#12573,#12574);
#10249=AXIS2_PLACEMENT_3D('',#16045,#12575,#12576);
#10250=AXIS2_PLACEMENT_3D('',#16046,#12577,#12578);
#10251=AXIS2_PLACEMENT_3D('',#16048,#12579,#12580);
#10252=AXIS2_PLACEMENT_3D('',#16051,#12582,#12583);
#10253=AXIS2_PLACEMENT_3D('',#16052,#12584,#12585);
#10254=AXIS2_PLACEMENT_3D('',#16054,#12586,#12587);
#10255=AXIS2_PLACEMENT_3D('',#16057,#12589,#12590);
#10256=AXIS2_PLACEMENT_3D('',#16058,#12591,#12592);
#10257=AXIS2_PLACEMENT_3D('',#16059,#12593,#12594);
#10258=AXIS2_PLACEMENT_3D('',#16060,#12595,#12596);
#10259=AXIS2_PLACEMENT_3D('',#16061,#12597,#12598);
#10260=AXIS2_PLACEMENT_3D('',#16148,#12600,#12601);
#10261=AXIS2_PLACEMENT_3D('',#16229,#12603,#12604);
#10262=AXIS2_PLACEMENT_3D('',#16231,#12605,#12606);
#10263=AXIS2_PLACEMENT_3D('',#16235,#12609,#12610);
#10264=AXIS2_PLACEMENT_3D('',#16318,#12611,#12612);
#10265=AXIS2_PLACEMENT_3D('',#16358,#12614,#12615);
#10266=AXIS2_PLACEMENT_3D('',#16398,#12617,#12618);
#10267=AXIS2_PLACEMENT_3D('',#16400,#12619,#12620);
#10268=AXIS2_PLACEMENT_3D('',#16404,#12623,#12624);
#10269=AXIS2_PLACEMENT_3D('',#16405,#12625,#12626);
#10270=AXIS2_PLACEMENT_3D('',#16406,#12627,#12628);
#10271=AXIS2_PLACEMENT_3D('',#16408,#12629,#12630);
#10272=AXIS2_PLACEMENT_3D('',#16411,#12631,#12632);
#10273=AXIS2_PLACEMENT_3D('',#16413,#12633,#12634);
#10274=AXIS2_PLACEMENT_3D('',#16415,#12635,#12636);
#10275=AXIS2_PLACEMENT_3D('',#16417,#12637,#12638);
#10276=AXIS2_PLACEMENT_3D('',#16419,#12639,#12640);
#10277=AXIS2_PLACEMENT_3D('',#16421,#12641,#12642);
#10278=AXIS2_PLACEMENT_3D('',#16423,#12643,#12644);
#10279=AXIS2_PLACEMENT_3D('',#16425,#12645,#12646);
#10280=AXIS2_PLACEMENT_3D('',#16427,#12647,#12648);
#10281=AXIS2_PLACEMENT_3D('',#16429,#12649,#12650);
#10282=AXIS2_PLACEMENT_3D('',#16431,#12651,#12652);
#10283=AXIS2_PLACEMENT_3D('',#16433,#12653,#12654);
#10284=AXIS2_PLACEMENT_3D('',#16435,#12655,#12656);
#10285=AXIS2_PLACEMENT_3D('',#16437,#12657,#12658);
#10286=AXIS2_PLACEMENT_3D('',#16439,#12659,#12660);
#10287=AXIS2_PLACEMENT_3D('',#16441,#12661,#12662);
#10288=AXIS2_PLACEMENT_3D('',#16443,#12663,#12664);
#10289=AXIS2_PLACEMENT_3D('',#16445,#12665,#12666);
#10290=AXIS2_PLACEMENT_3D('',#16447,#12667,#12668);
#10291=AXIS2_PLACEMENT_3D('',#16449,#12669,#12670);
#10292=AXIS2_PLACEMENT_3D('',#16451,#12671,#12672);
#10293=AXIS2_PLACEMENT_3D('',#16453,#12673,#12674);
#10294=AXIS2_PLACEMENT_3D('',#16455,#12675,#12676);
#10295=AXIS2_PLACEMENT_3D('',#16457,#12677,#12678);
#10296=AXIS2_PLACEMENT_3D('',#16459,#12679,#12680);
#10297=AXIS2_PLACEMENT_3D('',#16461,#12681,#12682);
#10298=AXIS2_PLACEMENT_3D('',#16463,#12683,#12684);
#10299=AXIS2_PLACEMENT_3D('',#16465,#12685,#12686);
#10300=AXIS2_PLACEMENT_3D('',#16467,#12687,#12688);
#10301=AXIS2_PLACEMENT_3D('',#16469,#12689,#12690);
#10302=AXIS2_PLACEMENT_3D('',#16471,#12691,#12692);
#10303=AXIS2_PLACEMENT_3D('',#16473,#12693,#12694);
#10304=AXIS2_PLACEMENT_3D('',#16475,#12695,#12696);
#10305=AXIS2_PLACEMENT_3D('',#16477,#12697,#12698);
#10306=AXIS2_PLACEMENT_3D('',#16479,#12699,#12700);
#10307=AXIS2_PLACEMENT_3D('',#16481,#12701,#12702);
#10308=AXIS2_PLACEMENT_3D('',#16483,#12703,#12704);
#10309=AXIS2_PLACEMENT_3D('',#16485,#12705,#12706);
#10310=AXIS2_PLACEMENT_3D('',#16487,#12707,#12708);
#10311=AXIS2_PLACEMENT_3D('',#16488,#12709,#12710);
#10312=AXIS2_PLACEMENT_3D('',#16489,#12711,#12712);
#10313=AXIS2_PLACEMENT_3D('',#16491,#12713,#12714);
#10314=AXIS2_PLACEMENT_3D('',#16493,#12716,#12717);
#10315=AXIS2_PLACEMENT_3D('',#16494,#12718,#12719);
#10316=AXIS2_PLACEMENT_3D('',#16496,#12720,#12721);
#10317=AXIS2_PLACEMENT_3D('',#16499,#12722,#12723);
#10318=AXIS2_PLACEMENT_3D('',#16501,#12724,#12725);
#10319=AXIS2_PLACEMENT_3D('',#16503,#12726,#12727);
#10320=AXIS2_PLACEMENT_3D('',#16505,#12728,#12729);
#10321=AXIS2_PLACEMENT_3D('',#16507,#12730,#12731);
#10322=AXIS2_PLACEMENT_3D('',#16509,#12732,#12733);
#10323=AXIS2_PLACEMENT_3D('',#16511,#12734,#12735);
#10324=AXIS2_PLACEMENT_3D('',#16513,#12736,#12737);
#10325=AXIS2_PLACEMENT_3D('',#16515,#12738,#12739);
#10326=AXIS2_PLACEMENT_3D('',#16517,#12740,#12741);
#10327=AXIS2_PLACEMENT_3D('',#16519,#12742,#12743);
#10328=AXIS2_PLACEMENT_3D('',#16521,#12744,#12745);
#10329=AXIS2_PLACEMENT_3D('',#16523,#12746,#12747);
#10330=AXIS2_PLACEMENT_3D('',#16525,#12748,#12749);
#10331=AXIS2_PLACEMENT_3D('',#16527,#12750,#12751);
#10332=AXIS2_PLACEMENT_3D('',#16529,#12752,#12753);
#10333=AXIS2_PLACEMENT_3D('',#16531,#12754,#12755);
#10334=AXIS2_PLACEMENT_3D('',#16533,#12756,#12757);
#10335=AXIS2_PLACEMENT_3D('',#16535,#12758,#12759);
#10336=AXIS2_PLACEMENT_3D('',#16537,#12760,#12761);
#10337=AXIS2_PLACEMENT_3D('',#16539,#12762,#12763);
#10338=AXIS2_PLACEMENT_3D('',#16541,#12764,#12765);
#10339=AXIS2_PLACEMENT_3D('',#16543,#12766,#12767);
#10340=AXIS2_PLACEMENT_3D('',#16545,#12768,#12769);
#10341=AXIS2_PLACEMENT_3D('',#16547,#12770,#12771);
#10342=AXIS2_PLACEMENT_3D('',#16549,#12772,#12773);
#10343=AXIS2_PLACEMENT_3D('',#16551,#12774,#12775);
#10344=AXIS2_PLACEMENT_3D('',#16553,#12776,#12777);
#10345=AXIS2_PLACEMENT_3D('',#16555,#12778,#12779);
#10346=AXIS2_PLACEMENT_3D('',#16557,#12780,#12781);
#10347=AXIS2_PLACEMENT_3D('',#16559,#12782,#12783);
#10348=AXIS2_PLACEMENT_3D('',#16561,#12784,#12785);
#10349=AXIS2_PLACEMENT_3D('',#16563,#12786,#12787);
#10350=AXIS2_PLACEMENT_3D('',#16565,#12788,#12789);
#10351=AXIS2_PLACEMENT_3D('',#16567,#12790,#12791);
#10352=AXIS2_PLACEMENT_3D('',#16569,#12792,#12793);
#10353=AXIS2_PLACEMENT_3D('',#16571,#12794,#12795);
#10354=AXIS2_PLACEMENT_3D('',#16573,#12796,#12797);
#10355=AXIS2_PLACEMENT_3D('',#16575,#12798,#12799);
#10356=AXIS2_PLACEMENT_3D('',#16576,#12800,#12801);
#10357=AXIS2_PLACEMENT_3D('',#16577,#12802,#12803);
#10358=AXIS2_PLACEMENT_3D('',#16579,#12804,#12805);
#10359=AXIS2_PLACEMENT_3D('',#16581,#12807,#12808);
#10360=AXIS2_PLACEMENT_3D('',#16582,#12809,#12810);
#10361=AXIS2_PLACEMENT_3D('',#16585,#12813,#12814);
#10362=AXIS2_PLACEMENT_3D('',#16587,#12816,#12817);
#10363=AXIS2_PLACEMENT_3D('',#16589,#12819,#12820);
#10364=AXIS2_PLACEMENT_3D('',#16591,#12822,#12823);
#10365=AXIS2_PLACEMENT_3D('',#16593,#12825,#12826);
#10366=AXIS2_PLACEMENT_3D('',#16595,#12828,#12829);
#10367=AXIS2_PLACEMENT_3D('',#16597,#12831,#12832);
#10368=AXIS2_PLACEMENT_3D('',#16599,#12834,#12835);
#10369=AXIS2_PLACEMENT_3D('',#16601,#12837,#12838);
#10370=AXIS2_PLACEMENT_3D('',#16603,#12840,#12841);
#10371=AXIS2_PLACEMENT_3D('',#16605,#12843,#12844);
#10372=AXIS2_PLACEMENT_3D('',#16607,#12846,#12847);
#10373=AXIS2_PLACEMENT_3D('',#16609,#12849,#12850);
#10374=AXIS2_PLACEMENT_3D('',#16611,#12852,#12853);
#10375=AXIS2_PLACEMENT_3D('',#16613,#12855,#12856);
#10376=AXIS2_PLACEMENT_3D('',#16615,#12858,#12859);
#10377=AXIS2_PLACEMENT_3D('',#16617,#12861,#12862);
#10378=AXIS2_PLACEMENT_3D('',#16619,#12864,#12865);
#10379=AXIS2_PLACEMENT_3D('',#16621,#12867,#12868);
#10380=AXIS2_PLACEMENT_3D('',#16623,#12870,#12871);
#10381=AXIS2_PLACEMENT_3D('',#16625,#12873,#12874);
#10382=AXIS2_PLACEMENT_3D('',#16627,#12876,#12877);
#10383=AXIS2_PLACEMENT_3D('',#16629,#12879,#12880);
#10384=AXIS2_PLACEMENT_3D('',#16631,#12882,#12883);
#10385=AXIS2_PLACEMENT_3D('',#16633,#12885,#12886);
#10386=AXIS2_PLACEMENT_3D('',#16635,#12888,#12889);
#10387=AXIS2_PLACEMENT_3D('',#16637,#12891,#12892);
#10388=AXIS2_PLACEMENT_3D('',#16639,#12894,#12895);
#10389=AXIS2_PLACEMENT_3D('',#16641,#12897,#12898);
#10390=AXIS2_PLACEMENT_3D('',#16643,#12900,#12901);
#10391=AXIS2_PLACEMENT_3D('',#16645,#12903,#12904);
#10392=AXIS2_PLACEMENT_3D('',#16647,#12906,#12907);
#10393=AXIS2_PLACEMENT_3D('',#16649,#12909,#12910);
#10394=AXIS2_PLACEMENT_3D('',#16651,#12912,#12913);
#10395=AXIS2_PLACEMENT_3D('',#16653,#12915,#12916);
#10396=AXIS2_PLACEMENT_3D('',#16655,#12918,#12919);
#10397=AXIS2_PLACEMENT_3D('',#16657,#12921,#12922);
#10398=AXIS2_PLACEMENT_3D('',#16659,#12924,#12925);
#10399=AXIS2_PLACEMENT_3D('',#16661,#12927,#12928);
#10400=AXIS2_PLACEMENT_3D('',#16662,#12929,#12930);
#10401=AXIS2_PLACEMENT_3D('',#16663,#12931,#12932);
#10402=AXIS2_PLACEMENT_3D('',#16664,#12933,#12934);
#10403=AXIS2_PLACEMENT_3D('',#16666,#12935,#12936);
#10404=AXIS2_PLACEMENT_3D('',#16669,#12938,#12939);
#10405=AXIS2_PLACEMENT_3D('',#16670,#12940,#12941);
#10406=AXIS2_PLACEMENT_3D('',#16671,#12942,#12943);
#10407=AXIS2_PLACEMENT_3D('',#16673,#12944,#12945);
#10408=AXIS2_PLACEMENT_3D('',#16675,#12946,#12947);
#10409=AXIS2_PLACEMENT_3D('',#16676,#12948,#12949);
#10410=AXIS2_PLACEMENT_3D('',#16678,#12950,#12951);
#10411=AXIS2_PLACEMENT_3D('',#16680,#12952,#12953);
#10412=AXIS2_PLACEMENT_3D('',#16681,#12954,#12955);
#10413=AXIS2_PLACEMENT_3D('',#16683,#12957,#12958);
#10414=AXIS2_PLACEMENT_3D('',#16686,#12960,#12961);
#10415=AXIS2_PLACEMENT_3D('',#16687,#12962,#12963);
#10416=AXIS2_PLACEMENT_3D('',#16688,#12964,#12965);
#10417=AXIS2_PLACEMENT_3D('',#16690,#12966,#12967);
#10418=AXIS2_PLACEMENT_3D('',#16692,#12969,#12970);
#10419=AXIS2_PLACEMENT_3D('',#16693,#12971,#12972);
#10420=AXIS2_PLACEMENT_3D('',#16694,#12973,#12974);
#10421=AXIS2_PLACEMENT_3D('',#16696,#12975,#12976);
#10422=AXIS2_PLACEMENT_3D('',#16699,#12978,#12979);
#10423=AXIS2_PLACEMENT_3D('',#16700,#12980,#12981);
#10424=AXIS2_PLACEMENT_3D('',#16702,#12982,#12983);
#10425=AXIS2_PLACEMENT_3D('',#16705,#12985,#12986);
#10426=AXIS2_PLACEMENT_3D('',#16706,#12987,#12988);
#10427=AXIS2_PLACEMENT_3D('',#16707,#12989,#12990);
#10428=AXIS2_PLACEMENT_3D('',#16708,#12991,#12992);
#10429=AXIS2_PLACEMENT_3D('',#16709,#12993,#12994);
#10430=AXIS2_PLACEMENT_3D('',#16711,#12995,#12996);
#10431=AXIS2_PLACEMENT_3D('',#16714,#12998,#12999);
#10432=AXIS2_PLACEMENT_3D('',#16715,#13000,#13001);
#10433=AXIS2_PLACEMENT_3D('',#16717,#13002,#13003);
#10434=AXIS2_PLACEMENT_3D('',#16720,#13005,#13006);
#10435=AXIS2_PLACEMENT_3D('',#16721,#13007,#13008);
#10436=AXIS2_PLACEMENT_3D('',#16722,#13009,#13010);
#10437=AXIS2_PLACEMENT_3D('',#16723,#13011,#13012);
#10438=AXIS2_PLACEMENT_3D('',#16724,#13013,#13014);
#10439=AXIS2_PLACEMENT_3D('',#16726,#13015,#13016);
#10440=AXIS2_PLACEMENT_3D('',#16729,#13018,#13019);
#10441=AXIS2_PLACEMENT_3D('',#16730,#13020,#13021);
#10442=AXIS2_PLACEMENT_3D('',#16731,#13022,#13023);
#10443=AXIS2_PLACEMENT_3D('',#16732,#13024,#13025);
#10444=AXIS2_PLACEMENT_3D('',#16733,#13026,#13027);
#10445=AXIS2_PLACEMENT_3D('',#16735,#13028,#13029);
#10446=AXIS2_PLACEMENT_3D('',#16738,#13031,#13032);
#10447=AXIS2_PLACEMENT_3D('',#16739,#13033,#13034);
#10448=AXIS2_PLACEMENT_3D('',#16740,#13035,#13036);
#10449=AXIS2_PLACEMENT_3D('',#16741,#13037,#13038);
#10450=AXIS2_PLACEMENT_3D('',#16742,#13039,#13040);
#10451=AXIS2_PLACEMENT_3D('',#16744,#13041,#13042);
#10452=AXIS2_PLACEMENT_3D('',#16747,#13044,#13045);
#10453=AXIS2_PLACEMENT_3D('',#16748,#13046,#13047);
#10454=AXIS2_PLACEMENT_3D('',#16750,#13048,#13049);
#10455=AXIS2_PLACEMENT_3D('',#16753,#13051,#13052);
#10456=AXIS2_PLACEMENT_3D('',#16754,#13053,#13054);
#10457=AXIS2_PLACEMENT_3D('',#16755,#13055,#13056);
#10458=AXIS2_PLACEMENT_3D('',#16756,#13057,#13058);
#10459=AXIS2_PLACEMENT_3D('',#16757,#13059,#13060);
#10460=AXIS2_PLACEMENT_3D('',#16844,#13062,#13063);
#10461=AXIS2_PLACEMENT_3D('',#16925,#13065,#13066);
#10462=AXIS2_PLACEMENT_3D('',#16927,#13067,#13068);
#10463=AXIS2_PLACEMENT_3D('',#16931,#13071,#13072);
#10464=AXIS2_PLACEMENT_3D('',#17014,#13073,#13074);
#10465=AXIS2_PLACEMENT_3D('',#17054,#13076,#13077);
#10466=AXIS2_PLACEMENT_3D('',#17094,#13079,#13080);
#10467=AXIS2_PLACEMENT_3D('',#17096,#13081,#13082);
#10468=AXIS2_PLACEMENT_3D('',#17100,#13085,#13086);
#10469=AXIS2_PLACEMENT_3D('',#17101,#13087,#13088);
#10470=AXIS2_PLACEMENT_3D('',#17102,#13089,#13090);
#10471=AXIS2_PLACEMENT_3D('',#17104,#13091,#13092);
#10472=AXIS2_PLACEMENT_3D('',#17107,#13093,#13094);
#10473=AXIS2_PLACEMENT_3D('',#17109,#13095,#13096);
#10474=AXIS2_PLACEMENT_3D('',#17111,#13097,#13098);
#10475=AXIS2_PLACEMENT_3D('',#17113,#13099,#13100);
#10476=AXIS2_PLACEMENT_3D('',#17115,#13101,#13102);
#10477=AXIS2_PLACEMENT_3D('',#17117,#13103,#13104);
#10478=AXIS2_PLACEMENT_3D('',#17119,#13105,#13106);
#10479=AXIS2_PLACEMENT_3D('',#17121,#13107,#13108);
#10480=AXIS2_PLACEMENT_3D('',#17123,#13109,#13110);
#10481=AXIS2_PLACEMENT_3D('',#17125,#13111,#13112);
#10482=AXIS2_PLACEMENT_3D('',#17127,#13113,#13114);
#10483=AXIS2_PLACEMENT_3D('',#17129,#13115,#13116);
#10484=AXIS2_PLACEMENT_3D('',#17131,#13117,#13118);
#10485=AXIS2_PLACEMENT_3D('',#17133,#13119,#13120);
#10486=AXIS2_PLACEMENT_3D('',#17135,#13121,#13122);
#10487=AXIS2_PLACEMENT_3D('',#17137,#13123,#13124);
#10488=AXIS2_PLACEMENT_3D('',#17139,#13125,#13126);
#10489=AXIS2_PLACEMENT_3D('',#17141,#13127,#13128);
#10490=AXIS2_PLACEMENT_3D('',#17143,#13129,#13130);
#10491=AXIS2_PLACEMENT_3D('',#17145,#13131,#13132);
#10492=AXIS2_PLACEMENT_3D('',#17147,#13133,#13134);
#10493=AXIS2_PLACEMENT_3D('',#17149,#13135,#13136);
#10494=AXIS2_PLACEMENT_3D('',#17151,#13137,#13138);
#10495=AXIS2_PLACEMENT_3D('',#17153,#13139,#13140);
#10496=AXIS2_PLACEMENT_3D('',#17155,#13141,#13142);
#10497=AXIS2_PLACEMENT_3D('',#17157,#13143,#13144);
#10498=AXIS2_PLACEMENT_3D('',#17159,#13145,#13146);
#10499=AXIS2_PLACEMENT_3D('',#17161,#13147,#13148);
#10500=AXIS2_PLACEMENT_3D('',#17163,#13149,#13150);
#10501=AXIS2_PLACEMENT_3D('',#17165,#13151,#13152);
#10502=AXIS2_PLACEMENT_3D('',#17167,#13153,#13154);
#10503=AXIS2_PLACEMENT_3D('',#17169,#13155,#13156);
#10504=AXIS2_PLACEMENT_3D('',#17171,#13157,#13158);
#10505=AXIS2_PLACEMENT_3D('',#17173,#13159,#13160);
#10506=AXIS2_PLACEMENT_3D('',#17175,#13161,#13162);
#10507=AXIS2_PLACEMENT_3D('',#17177,#13163,#13164);
#10508=AXIS2_PLACEMENT_3D('',#17179,#13165,#13166);
#10509=AXIS2_PLACEMENT_3D('',#17181,#13167,#13168);
#10510=AXIS2_PLACEMENT_3D('',#17183,#13169,#13170);
#10511=AXIS2_PLACEMENT_3D('',#17185,#13171,#13172);
#10512=AXIS2_PLACEMENT_3D('',#17187,#13173,#13174);
#10513=AXIS2_PLACEMENT_3D('',#17189,#13175,#13176);
#10514=AXIS2_PLACEMENT_3D('',#17191,#13177,#13178);
#10515=AXIS2_PLACEMENT_3D('',#17193,#13179,#13180);
#10516=AXIS2_PLACEMENT_3D('',#17195,#13181,#13182);
#10517=AXIS2_PLACEMENT_3D('',#17197,#13183,#13184);
#10518=AXIS2_PLACEMENT_3D('',#17199,#13185,#13186);
#10519=AXIS2_PLACEMENT_3D('',#17201,#13187,#13188);
#10520=AXIS2_PLACEMENT_3D('',#17203,#13189,#13190);
#10521=AXIS2_PLACEMENT_3D('',#17205,#13191,#13192);
#10522=AXIS2_PLACEMENT_3D('',#17207,#13193,#13194);
#10523=AXIS2_PLACEMENT_3D('',#17209,#13195,#13196);
#10524=AXIS2_PLACEMENT_3D('',#17211,#13197,#13198);
#10525=AXIS2_PLACEMENT_3D('',#17213,#13199,#13200);
#10526=AXIS2_PLACEMENT_3D('',#17215,#13201,#13202);
#10527=AXIS2_PLACEMENT_3D('',#17217,#13203,#13204);
#10528=AXIS2_PLACEMENT_3D('',#17219,#13205,#13206);
#10529=AXIS2_PLACEMENT_3D('',#17221,#13207,#13208);
#10530=AXIS2_PLACEMENT_3D('',#17223,#13209,#13210);
#10531=AXIS2_PLACEMENT_3D('',#17225,#13211,#13212);
#10532=AXIS2_PLACEMENT_3D('',#17227,#13213,#13214);
#10533=AXIS2_PLACEMENT_3D('',#17229,#13215,#13216);
#10534=AXIS2_PLACEMENT_3D('',#17231,#13217,#13218);
#10535=AXIS2_PLACEMENT_3D('',#17233,#13219,#13220);
#10536=AXIS2_PLACEMENT_3D('',#17235,#13221,#13222);
#10537=AXIS2_PLACEMENT_3D('',#17237,#13223,#13224);
#10538=AXIS2_PLACEMENT_3D('',#17239,#13225,#13226);
#10539=AXIS2_PLACEMENT_3D('',#17241,#13227,#13228);
#10540=AXIS2_PLACEMENT_3D('',#17243,#13229,#13230);
#10541=AXIS2_PLACEMENT_3D('',#17245,#13231,#13232);
#10542=AXIS2_PLACEMENT_3D('',#17247,#13233,#13234);
#10543=AXIS2_PLACEMENT_3D('',#17249,#13235,#13236);
#10544=AXIS2_PLACEMENT_3D('',#17251,#13237,#13238);
#10545=AXIS2_PLACEMENT_3D('',#17253,#13239,#13240);
#10546=AXIS2_PLACEMENT_3D('',#17255,#13241,#13242);
#10547=AXIS2_PLACEMENT_3D('',#17257,#13243,#13244);
#10548=AXIS2_PLACEMENT_3D('',#17259,#13245,#13246);
#10549=AXIS2_PLACEMENT_3D('',#17261,#13247,#13248);
#10550=AXIS2_PLACEMENT_3D('',#17263,#13249,#13250);
#10551=AXIS2_PLACEMENT_3D('',#17264,#13251,#13252);
#10552=AXIS2_PLACEMENT_3D('',#17265,#13253,#13254);
#10553=AXIS2_PLACEMENT_3D('',#17267,#13255,#13256);
#10554=AXIS2_PLACEMENT_3D('',#17269,#13258,#13259);
#10555=AXIS2_PLACEMENT_3D('',#17270,#13260,#13261);
#10556=AXIS2_PLACEMENT_3D('',#17272,#13262,#13263);
#10557=AXIS2_PLACEMENT_3D('',#17275,#13264,#13265);
#10558=AXIS2_PLACEMENT_3D('',#17277,#13266,#13267);
#10559=AXIS2_PLACEMENT_3D('',#17279,#13268,#13269);
#10560=AXIS2_PLACEMENT_3D('',#17281,#13270,#13271);
#10561=AXIS2_PLACEMENT_3D('',#17283,#13272,#13273);
#10562=AXIS2_PLACEMENT_3D('',#17285,#13274,#13275);
#10563=AXIS2_PLACEMENT_3D('',#17287,#13276,#13277);
#10564=AXIS2_PLACEMENT_3D('',#17289,#13278,#13279);
#10565=AXIS2_PLACEMENT_3D('',#17291,#13280,#13281);
#10566=AXIS2_PLACEMENT_3D('',#17293,#13282,#13283);
#10567=AXIS2_PLACEMENT_3D('',#17295,#13284,#13285);
#10568=AXIS2_PLACEMENT_3D('',#17297,#13286,#13287);
#10569=AXIS2_PLACEMENT_3D('',#17299,#13288,#13289);
#10570=AXIS2_PLACEMENT_3D('',#17301,#13290,#13291);
#10571=AXIS2_PLACEMENT_3D('',#17303,#13292,#13293);
#10572=AXIS2_PLACEMENT_3D('',#17305,#13294,#13295);
#10573=AXIS2_PLACEMENT_3D('',#17307,#13296,#13297);
#10574=AXIS2_PLACEMENT_3D('',#17309,#13298,#13299);
#10575=AXIS2_PLACEMENT_3D('',#17311,#13300,#13301);
#10576=AXIS2_PLACEMENT_3D('',#17313,#13302,#13303);
#10577=AXIS2_PLACEMENT_3D('',#17315,#13304,#13305);
#10578=AXIS2_PLACEMENT_3D('',#17317,#13306,#13307);
#10579=AXIS2_PLACEMENT_3D('',#17319,#13308,#13309);
#10580=AXIS2_PLACEMENT_3D('',#17321,#13310,#13311);
#10581=AXIS2_PLACEMENT_3D('',#17323,#13312,#13313);
#10582=AXIS2_PLACEMENT_3D('',#17325,#13314,#13315);
#10583=AXIS2_PLACEMENT_3D('',#17327,#13316,#13317);
#10584=AXIS2_PLACEMENT_3D('',#17329,#13318,#13319);
#10585=AXIS2_PLACEMENT_3D('',#17331,#13320,#13321);
#10586=AXIS2_PLACEMENT_3D('',#17333,#13322,#13323);
#10587=AXIS2_PLACEMENT_3D('',#17335,#13324,#13325);
#10588=AXIS2_PLACEMENT_3D('',#17337,#13326,#13327);
#10589=AXIS2_PLACEMENT_3D('',#17339,#13328,#13329);
#10590=AXIS2_PLACEMENT_3D('',#17341,#13330,#13331);
#10591=AXIS2_PLACEMENT_3D('',#17343,#13332,#13333);
#10592=AXIS2_PLACEMENT_3D('',#17345,#13334,#13335);
#10593=AXIS2_PLACEMENT_3D('',#17347,#13336,#13337);
#10594=AXIS2_PLACEMENT_3D('',#17349,#13338,#13339);
#10595=AXIS2_PLACEMENT_3D('',#17351,#13340,#13341);
#10596=AXIS2_PLACEMENT_3D('',#17353,#13342,#13343);
#10597=AXIS2_PLACEMENT_3D('',#17355,#13344,#13345);
#10598=AXIS2_PLACEMENT_3D('',#17357,#13346,#13347);
#10599=AXIS2_PLACEMENT_3D('',#17359,#13348,#13349);
#10600=AXIS2_PLACEMENT_3D('',#17361,#13350,#13351);
#10601=AXIS2_PLACEMENT_3D('',#17363,#13352,#13353);
#10602=AXIS2_PLACEMENT_3D('',#17365,#13354,#13355);
#10603=AXIS2_PLACEMENT_3D('',#17367,#13356,#13357);
#10604=AXIS2_PLACEMENT_3D('',#17369,#13358,#13359);
#10605=AXIS2_PLACEMENT_3D('',#17371,#13360,#13361);
#10606=AXIS2_PLACEMENT_3D('',#17373,#13362,#13363);
#10607=AXIS2_PLACEMENT_3D('',#17375,#13364,#13365);
#10608=AXIS2_PLACEMENT_3D('',#17377,#13366,#13367);
#10609=AXIS2_PLACEMENT_3D('',#17379,#13368,#13369);
#10610=AXIS2_PLACEMENT_3D('',#17381,#13370,#13371);
#10611=AXIS2_PLACEMENT_3D('',#17383,#13372,#13373);
#10612=AXIS2_PLACEMENT_3D('',#17385,#13374,#13375);
#10613=AXIS2_PLACEMENT_3D('',#17387,#13376,#13377);
#10614=AXIS2_PLACEMENT_3D('',#17389,#13378,#13379);
#10615=AXIS2_PLACEMENT_3D('',#17391,#13380,#13381);
#10616=AXIS2_PLACEMENT_3D('',#17393,#13382,#13383);
#10617=AXIS2_PLACEMENT_3D('',#17395,#13384,#13385);
#10618=AXIS2_PLACEMENT_3D('',#17397,#13386,#13387);
#10619=AXIS2_PLACEMENT_3D('',#17399,#13388,#13389);
#10620=AXIS2_PLACEMENT_3D('',#17401,#13390,#13391);
#10621=AXIS2_PLACEMENT_3D('',#17403,#13392,#13393);
#10622=AXIS2_PLACEMENT_3D('',#17405,#13394,#13395);
#10623=AXIS2_PLACEMENT_3D('',#17407,#13396,#13397);
#10624=AXIS2_PLACEMENT_3D('',#17409,#13398,#13399);
#10625=AXIS2_PLACEMENT_3D('',#17411,#13400,#13401);
#10626=AXIS2_PLACEMENT_3D('',#17413,#13402,#13403);
#10627=AXIS2_PLACEMENT_3D('',#17415,#13404,#13405);
#10628=AXIS2_PLACEMENT_3D('',#17417,#13406,#13407);
#10629=AXIS2_PLACEMENT_3D('',#17419,#13408,#13409);
#10630=AXIS2_PLACEMENT_3D('',#17421,#13410,#13411);
#10631=AXIS2_PLACEMENT_3D('',#17423,#13412,#13413);
#10632=AXIS2_PLACEMENT_3D('',#17425,#13414,#13415);
#10633=AXIS2_PLACEMENT_3D('',#17427,#13416,#13417);
#10634=AXIS2_PLACEMENT_3D('',#17429,#13418,#13419);
#10635=AXIS2_PLACEMENT_3D('',#17431,#13420,#13421);
#10636=AXIS2_PLACEMENT_3D('',#17432,#13422,#13423);
#10637=AXIS2_PLACEMENT_3D('',#17433,#13424,#13425);
#10638=AXIS2_PLACEMENT_3D('',#17435,#13426,#13427);
#10639=AXIS2_PLACEMENT_3D('',#17437,#13429,#13430);
#10640=AXIS2_PLACEMENT_3D('',#17438,#13431,#13432);
#10641=AXIS2_PLACEMENT_3D('',#17441,#13435,#13436);
#10642=AXIS2_PLACEMENT_3D('',#17443,#13438,#13439);
#10643=AXIS2_PLACEMENT_3D('',#17445,#13441,#13442);
#10644=AXIS2_PLACEMENT_3D('',#17447,#13444,#13445);
#10645=AXIS2_PLACEMENT_3D('',#17449,#13447,#13448);
#10646=AXIS2_PLACEMENT_3D('',#17451,#13450,#13451);
#10647=AXIS2_PLACEMENT_3D('',#17453,#13453,#13454);
#10648=AXIS2_PLACEMENT_3D('',#17455,#13456,#13457);
#10649=AXIS2_PLACEMENT_3D('',#17457,#13459,#13460);
#10650=AXIS2_PLACEMENT_3D('',#17459,#13462,#13463);
#10651=AXIS2_PLACEMENT_3D('',#17461,#13465,#13466);
#10652=AXIS2_PLACEMENT_3D('',#17463,#13468,#13469);
#10653=AXIS2_PLACEMENT_3D('',#17465,#13471,#13472);
#10654=AXIS2_PLACEMENT_3D('',#17467,#13474,#13475);
#10655=AXIS2_PLACEMENT_3D('',#17469,#13477,#13478);
#10656=AXIS2_PLACEMENT_3D('',#17471,#13480,#13481);
#10657=AXIS2_PLACEMENT_3D('',#17473,#13483,#13484);
#10658=AXIS2_PLACEMENT_3D('',#17475,#13486,#13487);
#10659=AXIS2_PLACEMENT_3D('',#17477,#13489,#13490);
#10660=AXIS2_PLACEMENT_3D('',#17479,#13492,#13493);
#10661=AXIS2_PLACEMENT_3D('',#17481,#13495,#13496);
#10662=AXIS2_PLACEMENT_3D('',#17483,#13498,#13499);
#10663=AXIS2_PLACEMENT_3D('',#17485,#13501,#13502);
#10664=AXIS2_PLACEMENT_3D('',#17487,#13504,#13505);
#10665=AXIS2_PLACEMENT_3D('',#17489,#13507,#13508);
#10666=AXIS2_PLACEMENT_3D('',#17491,#13510,#13511);
#10667=AXIS2_PLACEMENT_3D('',#17493,#13513,#13514);
#10668=AXIS2_PLACEMENT_3D('',#17495,#13516,#13517);
#10669=AXIS2_PLACEMENT_3D('',#17497,#13519,#13520);
#10670=AXIS2_PLACEMENT_3D('',#17499,#13522,#13523);
#10671=AXIS2_PLACEMENT_3D('',#17501,#13525,#13526);
#10672=AXIS2_PLACEMENT_3D('',#17503,#13528,#13529);
#10673=AXIS2_PLACEMENT_3D('',#17505,#13531,#13532);
#10674=AXIS2_PLACEMENT_3D('',#17507,#13534,#13535);
#10675=AXIS2_PLACEMENT_3D('',#17509,#13537,#13538);
#10676=AXIS2_PLACEMENT_3D('',#17511,#13540,#13541);
#10677=AXIS2_PLACEMENT_3D('',#17513,#13543,#13544);
#10678=AXIS2_PLACEMENT_3D('',#17515,#13546,#13547);
#10679=AXIS2_PLACEMENT_3D('',#17517,#13549,#13550);
#10680=AXIS2_PLACEMENT_3D('',#17519,#13552,#13553);
#10681=AXIS2_PLACEMENT_3D('',#17521,#13555,#13556);
#10682=AXIS2_PLACEMENT_3D('',#17523,#13558,#13559);
#10683=AXIS2_PLACEMENT_3D('',#17525,#13561,#13562);
#10684=AXIS2_PLACEMENT_3D('',#17527,#13564,#13565);
#10685=AXIS2_PLACEMENT_3D('',#17529,#13567,#13568);
#10686=AXIS2_PLACEMENT_3D('',#17531,#13570,#13571);
#10687=AXIS2_PLACEMENT_3D('',#17533,#13573,#13574);
#10688=AXIS2_PLACEMENT_3D('',#17535,#13576,#13577);
#10689=AXIS2_PLACEMENT_3D('',#17537,#13579,#13580);
#10690=AXIS2_PLACEMENT_3D('',#17539,#13582,#13583);
#10691=AXIS2_PLACEMENT_3D('',#17541,#13585,#13586);
#10692=AXIS2_PLACEMENT_3D('',#17543,#13588,#13589);
#10693=AXIS2_PLACEMENT_3D('',#17545,#13591,#13592);
#10694=AXIS2_PLACEMENT_3D('',#17547,#13594,#13595);
#10695=AXIS2_PLACEMENT_3D('',#17549,#13597,#13598);
#10696=AXIS2_PLACEMENT_3D('',#17551,#13600,#13601);
#10697=AXIS2_PLACEMENT_3D('',#17553,#13603,#13604);
#10698=AXIS2_PLACEMENT_3D('',#17555,#13606,#13607);
#10699=AXIS2_PLACEMENT_3D('',#17557,#13609,#13610);
#10700=AXIS2_PLACEMENT_3D('',#17559,#13612,#13613);
#10701=AXIS2_PLACEMENT_3D('',#17561,#13615,#13616);
#10702=AXIS2_PLACEMENT_3D('',#17563,#13618,#13619);
#10703=AXIS2_PLACEMENT_3D('',#17565,#13621,#13622);
#10704=AXIS2_PLACEMENT_3D('',#17567,#13624,#13625);
#10705=AXIS2_PLACEMENT_3D('',#17569,#13627,#13628);
#10706=AXIS2_PLACEMENT_3D('',#17571,#13630,#13631);
#10707=AXIS2_PLACEMENT_3D('',#17573,#13633,#13634);
#10708=AXIS2_PLACEMENT_3D('',#17575,#13636,#13637);
#10709=AXIS2_PLACEMENT_3D('',#17577,#13639,#13640);
#10710=AXIS2_PLACEMENT_3D('',#17579,#13642,#13643);
#10711=AXIS2_PLACEMENT_3D('',#17581,#13645,#13646);
#10712=AXIS2_PLACEMENT_3D('',#17583,#13648,#13649);
#10713=AXIS2_PLACEMENT_3D('',#17585,#13651,#13652);
#10714=AXIS2_PLACEMENT_3D('',#17587,#13654,#13655);
#10715=AXIS2_PLACEMENT_3D('',#17589,#13657,#13658);
#10716=AXIS2_PLACEMENT_3D('',#17591,#13660,#13661);
#10717=AXIS2_PLACEMENT_3D('',#17593,#13663,#13664);
#10718=AXIS2_PLACEMENT_3D('',#17595,#13666,#13667);
#10719=AXIS2_PLACEMENT_3D('',#17597,#13669,#13670);
#10720=AXIS2_PLACEMENT_3D('',#17598,#13671,#13672);
#10721=AXIS2_PLACEMENT_3D('',#17599,#13673,#13674);
#10722=AXIS2_PLACEMENT_3D('',#17601,#13675,#13676);
#10723=AXIS2_PLACEMENT_3D('',#17602,#13677,#13678);
#10724=AXIS2_PLACEMENT_3D('',#17604,#13679,#13680);
#10725=AXIS2_PLACEMENT_3D('',#17606,#13682,#13683);
#10726=AXIS2_PLACEMENT_3D('',#17608,#13684,#13685);
#10727=AXIS2_PLACEMENT_3D('',#17610,#13687,#13688);
#10728=AXIS2_PLACEMENT_3D('',#17612,#13689,#13690);
#10729=AXIS2_PLACEMENT_3D('',#17614,#13692,#13693);
#10730=AXIS2_PLACEMENT_3D('',#17616,#13694,#13695);
#10731=AXIS2_PLACEMENT_3D('',#17617,#13696,#13697);
#10732=AXIS2_PLACEMENT_3D('',#17619,#13698,#13699);
#10733=AXIS2_PLACEMENT_3D('',#17621,#13701,#13702);
#10734=AXIS2_PLACEMENT_3D('',#17623,#13703,#13704);
#10735=AXIS2_PLACEMENT_3D('',#17625,#13706,#13707);
#10736=AXIS2_PLACEMENT_3D('',#17627,#13708,#13709);
#10737=AXIS2_PLACEMENT_3D('',#17629,#13711,#13712);
#10738=AXIS2_PLACEMENT_3D('',#17630,#13713,#13714);
#10739=AXIS2_PLACEMENT_3D('',#17639,#13719,#13720);
#10740=AXIS2_PLACEMENT_3D('',#17645,#13724,#13725);
#10741=AXIS2_PLACEMENT_3D('',#17651,#13729,#13730);
#10742=AXIS2_PLACEMENT_3D('',#17657,#13734,#13735);
#10743=AXIS2_PLACEMENT_3D('',#17663,#13739,#13740);
#10744=AXIS2_PLACEMENT_3D('',#17666,#13743,#13744);
#10745=AXIS2_PLACEMENT_3D('',#17667,#13745,#13746);
#10746=AXIS2_PLACEMENT_3D('',#17668,#13747,#13748);
#10747=AXIS2_PLACEMENT_3D('',#17669,#13749,#13750);
#10748=AXIS2_PLACEMENT_3D('',#17670,#13751,#13752);
#10749=AXIS2_PLACEMENT_3D('',#17671,#13753,#13754);
#10750=AXIS2_PLACEMENT_3D('',#17672,#13755,#13756);
#10751=AXIS2_PLACEMENT_3D('',#17673,#13757,#13758);
#10752=AXIS2_PLACEMENT_3D('',#17674,#13759,#13760);
#10753=AXIS2_PLACEMENT_3D('',#17675,#13761,#13762);
#10754=AXIS2_PLACEMENT_3D('',#17676,#13763,#13764);
#10755=AXIS2_PLACEMENT_3D('',#17677,#13765,#13766);
#10756=AXIS2_PLACEMENT_3D('',#17678,#13767,#13768);
#10757=AXIS2_PLACEMENT_3D('',#17679,#13769,#13770);
#10758=AXIS2_PLACEMENT_3D('',#17680,#13771,#13772);
#10759=AXIS2_PLACEMENT_3D('',#17681,#13773,#13774);
#10760=AXIS2_PLACEMENT_3D('',#17682,#13775,#13776);
#10761=AXIS2_PLACEMENT_3D('',#17683,#13777,#13778);
#10762=AXIS2_PLACEMENT_3D('',#17684,#13779,#13780);
#10763=AXIS2_PLACEMENT_3D('',#17685,#13781,#13782);
#10764=AXIS2_PLACEMENT_3D('',#17686,#13783,#13784);
#10765=AXIS2_PLACEMENT_3D('',#17687,#13785,#13786);
#10766=AXIS2_PLACEMENT_3D('',#17688,#13787,#13788);
#10767=AXIS2_PLACEMENT_3D('',#17689,#13789,#13790);
#10768=AXIS2_PLACEMENT_3D('',#17690,#13791,#13792);
#10769=AXIS2_PLACEMENT_3D('',#17691,#13793,#13794);
#10770=AXIS2_PLACEMENT_3D('',#17692,#13795,#13796);
#10771=AXIS2_PLACEMENT_3D('',#17693,#13797,#13798);
#10772=AXIS2_PLACEMENT_3D('',#17694,#13799,#13800);
#10773=AXIS2_PLACEMENT_3D('',#17695,#13801,#13802);
#10774=AXIS2_PLACEMENT_3D('',#17696,#13803,#13804);
#10775=AXIS2_PLACEMENT_3D('',#17697,#13805,#13806);
#10776=AXIS2_PLACEMENT_3D('',#17698,#13807,#13808);
#10777=AXIS2_PLACEMENT_3D('',#17699,#13809,#13810);
#10778=AXIS2_PLACEMENT_3D('',#17700,#13811,#13812);
#10779=AXIS2_PLACEMENT_3D('',#17701,#13813,#13814);
#10780=AXIS2_PLACEMENT_3D('',#17702,#13815,#13816);
#10781=AXIS2_PLACEMENT_3D('',#17703,#13817,#13818);
#10782=AXIS2_PLACEMENT_3D('',#17704,#13819,#13820);
#10783=AXIS2_PLACEMENT_3D('',#17705,#13821,#13822);
#10784=AXIS2_PLACEMENT_3D('',#17706,#13823,#13824);
#10785=AXIS2_PLACEMENT_3D('',#17707,#13825,#13826);
#10786=AXIS2_PLACEMENT_3D('',#17708,#13827,#13828);
#10787=AXIS2_PLACEMENT_3D('',#17709,#13829,#13830);
#10788=AXIS2_PLACEMENT_3D('',#17710,#13831,#13832);
#10789=AXIS2_PLACEMENT_3D('',#17711,#13833,#13834);
#10790=AXIS2_PLACEMENT_3D('',#17712,#13835,#13836);
#10791=AXIS2_PLACEMENT_3D('',#17713,#13837,#13838);
#10792=AXIS2_PLACEMENT_3D('',#17714,#13839,#13840);
#10793=AXIS2_PLACEMENT_3D('',#17715,#13841,#13842);
#10794=AXIS2_PLACEMENT_3D('',#17716,#13843,#13844);
#10795=AXIS2_PLACEMENT_3D('',#17717,#13845,#13846);
#10796=AXIS2_PLACEMENT_3D('',#17718,#13847,#13848);
#10797=AXIS2_PLACEMENT_3D('',#17719,#13849,#13850);
#10798=AXIS2_PLACEMENT_3D('',#17720,#13851,#13852);
#10799=AXIS2_PLACEMENT_3D('',#17721,#13853,#13854);
#10800=AXIS2_PLACEMENT_3D('',#17722,#13855,#13856);
#10801=AXIS2_PLACEMENT_3D('',#17723,#13857,#13858);
#10802=AXIS2_PLACEMENT_3D('',#17724,#13859,#13860);
#10803=AXIS2_PLACEMENT_3D('',#17725,#13861,#13862);
#10804=AXIS2_PLACEMENT_3D('',#17726,#13863,#13864);
#10805=AXIS2_PLACEMENT_3D('',#17727,#13865,#13866);
#10806=AXIS2_PLACEMENT_3D('',#17728,#13867,#13868);
#10807=AXIS2_PLACEMENT_3D('',#17729,#13869,#13870);
#10808=AXIS2_PLACEMENT_3D('',#17730,#13871,#13872);
#10809=DIRECTION('axis',(0.,0.,1.));
#10810=DIRECTION('refdir',(1.,0.,0.));
#10811=DIRECTION('axis',(0.,0.,1.));
#10812=DIRECTION('refdir',(1.,0.,0.));
#10813=DIRECTION('axis',(0.,0.,1.));
#10814=DIRECTION('refdir',(1.,0.,0.));
#10815=DIRECTION('center_axis',(0.,0.,1.));
#10816=DIRECTION('ref_axis',(-1.,-1.22464679914735E-16,0.));
#10817=DIRECTION('',(0.,0.,1.));
#10818=DIRECTION('center_axis',(0.,0.,1.));
#10819=DIRECTION('ref_axis',(1.,0.,0.));
#10820=DIRECTION('',(0.,0.,1.));
#10821=DIRECTION('center_axis',(0.,0.,-1.));
#10822=DIRECTION('ref_axis',(1.,0.,0.));
#10823=DIRECTION('center_axis',(0.,0.,1.));
#10824=DIRECTION('ref_axis',(1.,0.,0.));
#10825=DIRECTION('',(0.,0.,1.));
#10826=DIRECTION('center_axis',(0.,0.,-1.));
#10827=DIRECTION('ref_axis',(1.,0.,0.));
#10828=DIRECTION('',(0.,0.,1.));
#10829=DIRECTION('center_axis',(0.,0.,1.));
#10830=DIRECTION('ref_axis',(1.,0.,0.));
#10831=DIRECTION('center_axis',(0.,0.,1.));
#10832=DIRECTION('ref_axis',(1.,0.,0.));
#10833=DIRECTION('',(0.,-1.,0.));
#10834=DIRECTION('',(-1.,0.,0.));
#10835=DIRECTION('',(0.,1.,0.));
#10836=DIRECTION('',(1.,0.,0.));
#10837=DIRECTION('center_axis',(0.,0.,1.));
#10838=DIRECTION('ref_axis',(1.,0.,0.));
#10839=DIRECTION('',(1.,0.,0.));
#10840=DIRECTION('center_axis',(0.,0.,1.));
#10841=DIRECTION('ref_axis',(1.,0.,0.));
#10842=DIRECTION('',(-1.,0.,0.));
#10843=DIRECTION('center_axis',(0.,0.,1.));
#10844=DIRECTION('ref_axis',(1.,0.,0.));
#10845=DIRECTION('',(1.,0.,0.));
#10846=DIRECTION('center_axis',(0.,0.,1.));
#10847=DIRECTION('ref_axis',(1.,0.,0.));
#10848=DIRECTION('',(-1.,0.,0.));
#10849=DIRECTION('center_axis',(0.,0.,1.));
#10850=DIRECTION('ref_axis',(1.,0.,0.));
#10851=DIRECTION('',(1.,0.,0.));
#10852=DIRECTION('center_axis',(0.,0.,1.));
#10853=DIRECTION('ref_axis',(1.,0.,0.));
#10854=DIRECTION('',(-1.,0.,0.));
#10855=DIRECTION('',(1.,0.,0.));
#10856=DIRECTION('',(-1.,0.,0.));
#10857=DIRECTION('center_axis',(0.,1.,0.));
#10858=DIRECTION('ref_axis',(-1.,0.,0.));
#10859=DIRECTION('',(1.,0.,0.));
#10860=DIRECTION('center_axis',(0.,-1.,0.));
#10861=DIRECTION('ref_axis',(1.,0.,0.));
#10862=DIRECTION('',(-1.,0.,0.));
#10863=DIRECTION('center_axis',(0.,0.,1.));
#10864=DIRECTION('ref_axis',(-1.,-1.22464679914735E-16,0.));
#10865=DIRECTION('',(0.,0.,1.));
#10866=DIRECTION('',(0.,0.,1.));
#10867=DIRECTION('center_axis',(0.,0.,-1.));
#10868=DIRECTION('ref_axis',(1.,0.,0.));
#10869=DIRECTION('center_axis',(0.,0.,1.));
#10870=DIRECTION('ref_axis',(1.,0.,0.));
#10871=DIRECTION('',(0.,0.,1.));
#10872=DIRECTION('center_axis',(0.,0.,-1.));
#10873=DIRECTION('ref_axis',(1.,0.,0.));
#10874=DIRECTION('',(0.,0.,1.));
#10875=DIRECTION('center_axis',(0.,1.,0.));
#10876=DIRECTION('ref_axis',(-1.,0.,0.));
#10877=DIRECTION('',(1.,0.,0.));
#10878=DIRECTION('center_axis',(0.,-1.,0.));
#10879=DIRECTION('ref_axis',(1.,0.,0.));
#10880=DIRECTION('',(-1.,0.,0.));
#10881=DIRECTION('center_axis',(0.,0.,1.));
#10882=DIRECTION('ref_axis',(-1.,-1.22464679914735E-16,0.));
#10883=DIRECTION('',(0.,0.,-1.));
#10884=DIRECTION('center_axis',(0.,0.,-1.));
#10885=DIRECTION('ref_axis',(1.,0.,0.));
#10886=DIRECTION('',(0.,0.,1.));
#10887=DIRECTION('',(0.,0.,1.));
#10888=DIRECTION('center_axis',(0.,0.,-1.));
#10889=DIRECTION('ref_axis',(1.,0.,0.));
#10890=DIRECTION('',(0.,0.,1.));
#10891=DIRECTION('center_axis',(0.,0.,-1.));
#10892=DIRECTION('ref_axis',(1.,0.,0.));
#10893=DIRECTION('center_axis',(0.,0.,1.));
#10894=DIRECTION('ref_axis',(1.,0.,0.));
#10895=DIRECTION('',(0.,0.,1.));
#10896=DIRECTION('center_axis',(0.,0.,-1.));
#10897=DIRECTION('ref_axis',(1.,0.,0.));
#10898=DIRECTION('',(0.,0.,1.));
#10899=DIRECTION('center_axis',(0.,1.,0.));
#10900=DIRECTION('ref_axis',(-1.,0.,0.));
#10901=DIRECTION('',(1.,0.,0.));
#10902=DIRECTION('center_axis',(0.,-1.,0.));
#10903=DIRECTION('ref_axis',(1.,0.,0.));
#10904=DIRECTION('',(-1.,0.,0.));
#10905=DIRECTION('center_axis',(0.,0.,1.));
#10906=DIRECTION('ref_axis',(-1.,-1.22464679914735E-16,0.));
#10907=DIRECTION('',(0.,0.,-1.));
#10908=DIRECTION('center_axis',(0.,0.,-1.));
#10909=DIRECTION('ref_axis',(1.,0.,0.));
#10910=DIRECTION('',(0.,0.,1.));
#10911=DIRECTION('',(0.,0.,1.));
#10912=DIRECTION('center_axis',(0.,0.,-1.));
#10913=DIRECTION('ref_axis',(1.,0.,0.));
#10914=DIRECTION('',(0.,0.,1.));
#10915=DIRECTION('center_axis',(0.,0.,-1.));
#10916=DIRECTION('ref_axis',(1.,0.,0.));
#10917=DIRECTION('center_axis',(0.,0.,1.));
#10918=DIRECTION('ref_axis',(1.,0.,0.));
#10919=DIRECTION('',(0.,0.,1.));
#10920=DIRECTION('center_axis',(0.,0.,-1.));
#10921=DIRECTION('ref_axis',(1.,0.,0.));
#10922=DIRECTION('',(0.,0.,1.));
#10923=DIRECTION('center_axis',(0.,1.,0.));
#10924=DIRECTION('ref_axis',(-1.,0.,0.));
#10925=DIRECTION('',(1.,0.,0.));
#10926=DIRECTION('center_axis',(0.,-1.,0.));
#10927=DIRECTION('ref_axis',(1.,0.,0.));
#10928=DIRECTION('',(-1.,0.,0.));
#10929=DIRECTION('center_axis',(0.,0.,1.));
#10930=DIRECTION('ref_axis',(-1.,5.66553889764798E-16,0.));
#10931=DIRECTION('center_axis',(0.,0.,-1.));
#10932=DIRECTION('ref_axis',(1.,0.,0.));
#10933=DIRECTION('center_axis',(0.,0.,1.));
#10934=DIRECTION('ref_axis',(1.,0.,0.));
#10935=DIRECTION('center_axis',(0.,0.,1.));
#10936=DIRECTION('ref_axis',(1.,0.,0.));
#10937=DIRECTION('center_axis',(0.,0.,1.));
#10938=DIRECTION('ref_axis',(1.,0.,0.));
#10939=DIRECTION('center_axis',(0.,0.,1.));
#10940=DIRECTION('ref_axis',(1.,0.,0.));
#10941=DIRECTION('',(0.,0.,1.));
#10942=DIRECTION('center_axis',(0.,0.,-1.));
#10943=DIRECTION('ref_axis',(1.,0.,0.));
#10944=DIRECTION('center_axis',(0.,0.,1.));
#10945=DIRECTION('ref_axis',(1.,0.,0.));
#10946=DIRECTION('center_axis',(0.,0.,1.));
#10947=DIRECTION('ref_axis',(1.,0.,0.));
#10948=DIRECTION('center_axis',(0.,0.,1.));
#10949=DIRECTION('ref_axis',(1.,0.,0.));
#10950=DIRECTION('',(0.,0.,1.));
#10951=DIRECTION('center_axis',(0.,0.,-1.));
#10952=DIRECTION('ref_axis',(1.,0.,0.));
#10953=DIRECTION('center_axis',(0.,0.,1.));
#10954=DIRECTION('ref_axis',(1.,0.,0.));
#10955=DIRECTION('center_axis',(0.,0.,1.));
#10956=DIRECTION('ref_axis',(-1.,-3.21624529935327E-16,0.));
#10957=DIRECTION('center_axis',(0.,0.,-1.));
#10958=DIRECTION('ref_axis',(1.,0.,0.));
#10959=DIRECTION('center_axis',(0.,0.,1.));
#10960=DIRECTION('ref_axis',(1.,0.,0.));
#10961=DIRECTION('center_axis',(0.,0.,1.));
#10962=DIRECTION('ref_axis',(1.,0.,0.));
#10963=DIRECTION('center_axis',(0.,1.,0.));
#10964=DIRECTION('ref_axis',(-1.,0.,0.));
#10965=DIRECTION('',(0.,0.,1.));
#10966=DIRECTION('',(-1.,0.,0.));
#10967=DIRECTION('',(0.,0.,1.));
#10968=DIRECTION('center_axis',(1.,0.,0.));
#10969=DIRECTION('ref_axis',(0.,1.,0.));
#10970=DIRECTION('',(0.,1.,0.));
#10971=DIRECTION('',(0.,0.,1.));
#10972=DIRECTION('center_axis',(0.,-1.,0.));
#10973=DIRECTION('ref_axis',(1.,0.,0.));
#10974=DIRECTION('',(1.,0.,0.));
#10975=DIRECTION('',(0.,0.,1.));
#10976=DIRECTION('center_axis',(-1.,0.,0.));
#10977=DIRECTION('ref_axis',(0.,-1.,0.));
#10978=DIRECTION('',(0.,-1.,0.));
#10979=DIRECTION('center_axis',(0.,0.,1.));
#10980=DIRECTION('ref_axis',(1.,0.,0.));
#10981=DIRECTION('axis',(0.,0.,1.));
#10982=DIRECTION('refdir',(1.,0.,0.));
#10983=DIRECTION('center_axis',(0.,1.,0.));
#10984=DIRECTION('ref_axis',(-1.,0.,0.));
#10985=DIRECTION('',(-1.,0.,0.));
#10986=DIRECTION('',(0.,0.,1.));
#10987=DIRECTION('',(-1.,0.,0.));
#10988=DIRECTION('',(0.,0.,1.));
#10989=DIRECTION('center_axis',(1.,0.,0.));
#10990=DIRECTION('ref_axis',(0.,1.,0.));
#10991=DIRECTION('',(0.,1.,0.));
#10992=DIRECTION('',(0.,1.,0.));
#10993=DIRECTION('',(0.,0.,1.));
#10994=DIRECTION('center_axis',(0.,-1.,0.));
#10995=DIRECTION('ref_axis',(1.,0.,0.));
#10996=DIRECTION('',(1.,0.,0.));
#10997=DIRECTION('',(1.,0.,0.));
#10998=DIRECTION('',(0.,0.,1.));
#10999=DIRECTION('center_axis',(-1.,0.,0.));
#11000=DIRECTION('ref_axis',(0.,-1.,0.));
#11001=DIRECTION('',(0.,-1.,0.));
#11002=DIRECTION('',(0.,-1.,0.));
#11003=DIRECTION('center_axis',(0.,0.,1.));
#11004=DIRECTION('ref_axis',(1.,0.,0.));
#11005=DIRECTION('center_axis',(0.,0.,1.));
#11006=DIRECTION('ref_axis',(1.,0.,0.));
#11007=DIRECTION('axis',(0.,0.,1.));
#11008=DIRECTION('refdir',(1.,0.,0.));
#11009=DIRECTION('center_axis',(0.,1.,0.));
#11010=DIRECTION('ref_axis',(-1.,0.,0.));
#11011=DIRECTION('',(-1.,0.,0.));
#11012=DIRECTION('',(0.,0.,1.));
#11013=DIRECTION('',(-1.,0.,0.));
#11014=DIRECTION('',(0.,0.,1.));
#11015=DIRECTION('center_axis',(1.,0.,0.));
#11016=DIRECTION('ref_axis',(0.,1.,0.));
#11017=DIRECTION('',(0.,1.,0.));
#11018=DIRECTION('',(0.,1.,0.));
#11019=DIRECTION('',(0.,0.,1.));
#11020=DIRECTION('center_axis',(0.,-1.,0.));
#11021=DIRECTION('ref_axis',(1.,0.,0.));
#11022=DIRECTION('',(1.,0.,0.));
#11023=DIRECTION('',(1.,0.,0.));
#11024=DIRECTION('',(0.,0.,1.));
#11025=DIRECTION('center_axis',(-1.,0.,0.));
#11026=DIRECTION('ref_axis',(0.,-1.,0.));
#11027=DIRECTION('',(0.,-1.,0.));
#11028=DIRECTION('',(0.,-1.,0.));
#11029=DIRECTION('center_axis',(0.,0.,1.));
#11030=DIRECTION('ref_axis',(1.,0.,0.));
#11031=DIRECTION('center_axis',(0.,0.,1.));
#11032=DIRECTION('ref_axis',(1.,0.,0.));
#11033=DIRECTION('axis',(0.,0.,1.));
#11034=DIRECTION('refdir',(1.,0.,0.));
#11035=DIRECTION('center_axis',(0.,1.,0.));
#11036=DIRECTION('ref_axis',(1.,0.,0.));
#11037=DIRECTION('center_axis',(0.,1.,0.));
#11038=DIRECTION('ref_axis',(1.,0.,0.));
#11039=DIRECTION('',(0.,1.,0.));
#11040=DIRECTION('center_axis',(0.,-1.,0.));
#11041=DIRECTION('ref_axis',(1.,0.,0.));
#11042=DIRECTION('center_axis',(0.,1.,0.));
#11043=DIRECTION('ref_axis',(1.,0.,0.));
#11044=DIRECTION('center_axis',(0.,1.,0.));
#11045=DIRECTION('ref_axis',(1.,0.,0.));
#11046=DIRECTION('',(0.,1.,0.));
#11047=DIRECTION('center_axis',(0.,-1.,0.));
#11048=DIRECTION('ref_axis',(1.,0.,0.));
#11049=DIRECTION('center_axis',(0.,1.,0.));
#11050=DIRECTION('ref_axis',(1.,0.,0.));
#11051=DIRECTION('center_axis',(0.,1.,0.));
#11052=DIRECTION('ref_axis',(1.,0.,0.));
#11053=DIRECTION('',(0.,1.,0.));
#11054=DIRECTION('center_axis',(0.,-1.,0.));
#11055=DIRECTION('ref_axis',(1.,0.,0.));
#11056=DIRECTION('center_axis',(0.,1.,0.));
#11057=DIRECTION('ref_axis',(1.,0.,0.));
#11058=DIRECTION('center_axis',(0.,1.,0.));
#11059=DIRECTION('ref_axis',(1.,0.,0.));
#11060=DIRECTION('',(0.,1.,0.));
#11061=DIRECTION('center_axis',(0.,-1.,0.));
#11062=DIRECTION('ref_axis',(1.,0.,0.));
#11063=DIRECTION('center_axis',(0.,1.,0.));
#11064=DIRECTION('ref_axis',(1.,0.,0.));
#11065=DIRECTION('center_axis',(0.,1.,0.));
#11066=DIRECTION('ref_axis',(1.,0.,0.));
#11067=DIRECTION('',(0.,1.,0.));
#11068=DIRECTION('center_axis',(0.,-1.,0.));
#11069=DIRECTION('ref_axis',(1.,0.,0.));
#11070=DIRECTION('center_axis',(0.,0.,1.));
#11071=DIRECTION('ref_axis',(1.,0.,0.));
#11072=DIRECTION('center_axis',(0.,0.,1.));
#11073=DIRECTION('ref_axis',(1.,0.,0.));
#11074=DIRECTION('',(0.,0.,1.));
#11075=DIRECTION('center_axis',(0.,0.,-1.));
#11076=DIRECTION('ref_axis',(1.,0.,0.));
#11077=DIRECTION('center_axis',(0.,0.,1.));
#11078=DIRECTION('ref_axis',(1.,0.,0.));
#11079=DIRECTION('center_axis',(0.,0.,1.));
#11080=DIRECTION('ref_axis',(1.,0.,0.));
#11081=DIRECTION('',(0.,0.,1.));
#11082=DIRECTION('center_axis',(0.,0.,-1.));
#11083=DIRECTION('ref_axis',(1.,0.,0.));
#11084=DIRECTION('center_axis',(0.,0.,1.));
#11085=DIRECTION('ref_axis',(1.,0.,0.));
#11086=DIRECTION('center_axis',(0.,0.,1.));
#11087=DIRECTION('ref_axis',(1.,0.,0.));
#11088=DIRECTION('',(0.,0.,1.));
#11089=DIRECTION('center_axis',(0.,0.,-1.));
#11090=DIRECTION('ref_axis',(1.,0.,0.));
#11091=DIRECTION('center_axis',(0.,0.,1.));
#11092=DIRECTION('ref_axis',(1.,0.,0.));
#11093=DIRECTION('center_axis',(0.,0.,1.));
#11094=DIRECTION('ref_axis',(1.,0.,0.));
#11095=DIRECTION('',(0.,0.,1.));
#11096=DIRECTION('center_axis',(0.,0.,-1.));
#11097=DIRECTION('ref_axis',(1.,0.,0.));
#11098=DIRECTION('center_axis',(0.,0.,1.));
#11099=DIRECTION('ref_axis',(1.,0.,0.));
#11100=DIRECTION('',(0.,1.,0.));
#11101=DIRECTION('',(-1.,0.,0.));
#11102=DIRECTION('',(0.,1.,0.));
#11103=DIRECTION('',(1.,0.,0.));
#11104=DIRECTION('center_axis',(0.,0.,1.));
#11105=DIRECTION('ref_axis',(1.,0.,0.));
#11106=DIRECTION('',(0.,-1.,0.));
#11107=DIRECTION('',(1.,0.,0.));
#11108=DIRECTION('',(0.,1.,0.));
#11109=DIRECTION('',(-1.,0.,0.));
#11110=DIRECTION('center_axis',(-1.,0.,0.));
#11111=DIRECTION('ref_axis',(0.,0.,1.));
#11112=DIRECTION('',(0.,0.,-1.));
#11113=DIRECTION('',(0.,0.,1.));
#11114=DIRECTION('',(0.,1.,0.));
#11115=DIRECTION('center_axis',(1.,0.,0.));
#11116=DIRECTION('ref_axis',(0.,0.,-1.));
#11117=DIRECTION('',(0.,0.,1.));
#11118=DIRECTION('',(0.,1.,0.));
#11119=DIRECTION('',(0.,0.,-1.));
#11120=DIRECTION('center_axis',(0.,-1.,0.));
#11121=DIRECTION('ref_axis',(1.,0.,0.));
#11122=DIRECTION('',(0.,0.,1.));
#11123=DIRECTION('',(1.,0.,0.));
#11124=DIRECTION('',(0.,0.,1.));
#11125=DIRECTION('',(1.,0.,0.));
#11126=DIRECTION('center_axis',(1.,0.,0.));
#11127=DIRECTION('ref_axis',(0.,1.,0.));
#11128=DIRECTION('',(0.,0.,1.));
#11129=DIRECTION('',(0.,1.,0.));
#11130=DIRECTION('center_axis',(0.,1.,0.));
#11131=DIRECTION('ref_axis',(-1.,0.,0.));
#11132=DIRECTION('',(0.,0.,1.));
#11133=DIRECTION('',(-1.,0.,0.));
#11134=DIRECTION('',(-1.,0.,0.));
#11135=DIRECTION('center_axis',(-1.,0.,0.));
#11136=DIRECTION('ref_axis',(0.,-1.,0.));
#11137=DIRECTION('',(0.,-1.,0.));
#11138=DIRECTION('center_axis',(0.,0.,1.));
#11139=DIRECTION('ref_axis',(1.,0.,0.));
#11140=DIRECTION('center_axis',(0.,0.,1.));
#11141=DIRECTION('ref_axis',(1.,0.,0.));
#11142=DIRECTION('axis',(0.,0.,1.));
#11143=DIRECTION('refdir',(1.,0.,0.));
#11144=DIRECTION('center_axis',(0.,1.,0.));
#11145=DIRECTION('ref_axis',(1.,0.,0.));
#11146=DIRECTION('center_axis',(0.,-1.,0.));
#11147=DIRECTION('ref_axis',(1.,0.,0.));
#11148=DIRECTION('',(0.,-1.,0.));
#11149=DIRECTION('center_axis',(0.,-1.,0.));
#11150=DIRECTION('ref_axis',(1.,0.,0.));
#11151=DIRECTION('center_axis',(0.,1.,0.));
#11152=DIRECTION('ref_axis',(1.,0.,0.));
#11153=DIRECTION('center_axis',(0.,1.,0.));
#11154=DIRECTION('ref_axis',(1.,0.,0.));
#11155=DIRECTION('',(0.,-1.,0.));
#11156=DIRECTION('center_axis',(0.,1.,0.));
#11157=DIRECTION('ref_axis',(1.,0.,0.));
#11158=DIRECTION('center_axis',(0.,1.,0.));
#11159=DIRECTION('ref_axis',(1.,0.,0.));
#11160=DIRECTION('center_axis',(0.,1.,0.));
#11161=DIRECTION('ref_axis',(1.,0.,0.));
#11162=DIRECTION('axis',(0.,0.,1.));
#11163=DIRECTION('refdir',(1.,0.,0.));
#11164=DIRECTION('center_axis',(0.,1.,0.));
#11165=DIRECTION('ref_axis',(0.707106781186546,0.,0.707106781186549));
#11166=DIRECTION('',(0.,1.,0.));
#11167=DIRECTION('center_axis',(0.,1.,0.));
#11168=DIRECTION('ref_axis',(1.,0.,0.));
#11169=DIRECTION('',(0.,-1.,0.));
#11170=DIRECTION('center_axis',(0.,-1.,0.));
#11171=DIRECTION('ref_axis',(1.,0.,0.));
#11172=DIRECTION('center_axis',(0.,1.,0.));
#11173=DIRECTION('ref_axis',(0.707106781186547,0.,-0.707106781186548));
#11174=DIRECTION('',(0.,1.,0.));
#11175=DIRECTION('center_axis',(0.,1.,0.));
#11176=DIRECTION('ref_axis',(1.,0.,0.));
#11177=DIRECTION('',(0.,-1.,0.));
#11178=DIRECTION('center_axis',(0.,-1.,0.));
#11179=DIRECTION('ref_axis',(1.,0.,0.));
#11180=DIRECTION('center_axis',(0.,1.,0.));
#11181=DIRECTION('ref_axis',(-0.707106781186552,0.,-0.707106781186543));
#11182=DIRECTION('',(0.,1.,0.));
#11183=DIRECTION('center_axis',(0.,1.,0.));
#11184=DIRECTION('ref_axis',(1.,0.,0.));
#11185=DIRECTION('',(0.,-1.,0.));
#11186=DIRECTION('center_axis',(0.,-1.,0.));
#11187=DIRECTION('ref_axis',(1.,0.,0.));
#11188=DIRECTION('center_axis',(0.,1.,0.));
#11189=DIRECTION('ref_axis',(-0.707106781186546,0.,0.707106781186549));
#11190=DIRECTION('',(0.,1.,0.));
#11191=DIRECTION('center_axis',(0.,1.,0.));
#11192=DIRECTION('ref_axis',(1.,0.,0.));
#11193=DIRECTION('',(0.,-1.,0.));
#11194=DIRECTION('center_axis',(0.,-1.,0.));
#11195=DIRECTION('ref_axis',(1.,0.,0.));
#11196=DIRECTION('center_axis',(0.,1.,0.));
#11197=DIRECTION('ref_axis',(1.,0.,0.));
#11198=DIRECTION('center_axis',(0.,1.,0.));
#11199=DIRECTION('ref_axis',(1.,0.,0.));
#11200=DIRECTION('center_axis',(0.,1.,0.));
#11201=DIRECTION('ref_axis',(1.,0.,0.));
#11202=DIRECTION('center_axis',(0.,1.,0.));
#11203=DIRECTION('ref_axis',(1.,0.,0.));
#11204=DIRECTION('center_axis',(0.,1.,0.));
#11205=DIRECTION('ref_axis',(1.,0.,0.));
#11206=DIRECTION('center_axis',(0.,-1.,0.));
#11207=DIRECTION('ref_axis',(1.,0.,0.));
#11208=DIRECTION('center_axis',(0.,1.,0.));
#11209=DIRECTION('ref_axis',(1.,0.,0.));
#11210=DIRECTION('center_axis',(0.,1.,0.));
#11211=DIRECTION('ref_axis',(1.,0.,0.));
#11212=DIRECTION('center_axis',(0.,1.,0.));
#11213=DIRECTION('ref_axis',(1.,0.,0.));
#11214=DIRECTION('center_axis',(0.,1.,0.));
#11215=DIRECTION('ref_axis',(1.,0.,0.));
#11216=DIRECTION('center_axis',(0.,1.,0.));
#11217=DIRECTION('ref_axis',(1.,0.,0.));
#11218=DIRECTION('center_axis',(0.,1.,0.));
#11219=DIRECTION('ref_axis',(1.,0.,0.));
#11220=DIRECTION('center_axis',(0.,1.,0.));
#11221=DIRECTION('ref_axis',(-1.,0.,-1.22464679914735E-16));
#11222=DIRECTION('center_axis',(0.,1.,0.));
#11223=DIRECTION('ref_axis',(1.,0.,0.));
#11224=DIRECTION('center_axis',(0.,1.,0.));
#11225=DIRECTION('ref_axis',(1.,0.,0.));
#11226=DIRECTION('center_axis',(0.,1.,0.));
#11227=DIRECTION('ref_axis',(1.,0.,0.));
#11228=DIRECTION('',(0.,-1.,0.));
#11229=DIRECTION('center_axis',(0.,-1.,0.));
#11230=DIRECTION('ref_axis',(1.,0.,0.));
#11231=DIRECTION('center_axis',(0.,1.,0.));
#11232=DIRECTION('ref_axis',(1.,0.,0.));
#11233=DIRECTION('center_axis',(0.,-1.,0.));
#11234=DIRECTION('ref_axis',(1.,0.,0.));
#11235=DIRECTION('center_axis',(0.,1.,0.));
#11236=DIRECTION('ref_axis',(1.,0.,0.));
#11237=DIRECTION('',(0.,-1.,0.));
#11238=DIRECTION('center_axis',(0.,1.,0.));
#11239=DIRECTION('ref_axis',(1.,0.,0.));
#11240=DIRECTION('axis',(0.,0.,1.));
#11241=DIRECTION('refdir',(1.,0.,0.));
#11242=DIRECTION('center_axis',(0.,1.,0.));
#11243=DIRECTION('ref_axis',(0.707106781186546,0.,0.707106781186549));
#11244=DIRECTION('',(0.,1.,0.));
#11245=DIRECTION('center_axis',(0.,1.,0.));
#11246=DIRECTION('ref_axis',(1.,0.,0.));
#11247=DIRECTION('',(0.,-1.,0.));
#11248=DIRECTION('center_axis',(0.,-1.,0.));
#11249=DIRECTION('ref_axis',(1.,0.,0.));
#11250=DIRECTION('center_axis',(0.,1.,0.));
#11251=DIRECTION('ref_axis',(0.707106781186547,0.,-0.707106781186548));
#11252=DIRECTION('',(0.,1.,0.));
#11253=DIRECTION('center_axis',(0.,1.,0.));
#11254=DIRECTION('ref_axis',(1.,0.,0.));
#11255=DIRECTION('',(0.,-1.,0.));
#11256=DIRECTION('center_axis',(0.,-1.,0.));
#11257=DIRECTION('ref_axis',(1.,0.,0.));
#11258=DIRECTION('center_axis',(0.,1.,0.));
#11259=DIRECTION('ref_axis',(-0.707106781186552,0.,-0.707106781186543));
#11260=DIRECTION('',(0.,1.,0.));
#11261=DIRECTION('center_axis',(0.,1.,0.));
#11262=DIRECTION('ref_axis',(1.,0.,0.));
#11263=DIRECTION('',(0.,-1.,0.));
#11264=DIRECTION('center_axis',(0.,-1.,0.));
#11265=DIRECTION('ref_axis',(1.,0.,0.));
#11266=DIRECTION('center_axis',(0.,1.,0.));
#11267=DIRECTION('ref_axis',(-0.707106781186546,0.,0.707106781186549));
#11268=DIRECTION('',(0.,1.,0.));
#11269=DIRECTION('center_axis',(0.,1.,0.));
#11270=DIRECTION('ref_axis',(1.,0.,0.));
#11271=DIRECTION('',(0.,-1.,0.));
#11272=DIRECTION('center_axis',(0.,-1.,0.));
#11273=DIRECTION('ref_axis',(1.,0.,0.));
#11274=DIRECTION('center_axis',(0.,1.,0.));
#11275=DIRECTION('ref_axis',(1.,0.,0.));
#11276=DIRECTION('center_axis',(0.,1.,0.));
#11277=DIRECTION('ref_axis',(1.,0.,0.));
#11278=DIRECTION('center_axis',(0.,1.,0.));
#11279=DIRECTION('ref_axis',(1.,0.,0.));
#11280=DIRECTION('center_axis',(0.,1.,0.));
#11281=DIRECTION('ref_axis',(1.,0.,0.));
#11282=DIRECTION('center_axis',(0.,1.,0.));
#11283=DIRECTION('ref_axis',(1.,0.,0.));
#11284=DIRECTION('center_axis',(0.,1.,0.));
#11285=DIRECTION('ref_axis',(1.,0.,0.));
#11286=DIRECTION('center_axis',(0.,1.,0.));
#11287=DIRECTION('ref_axis',(1.,0.,0.));
#11288=DIRECTION('center_axis',(0.,1.,0.));
#11289=DIRECTION('ref_axis',(1.,0.,0.));
#11290=DIRECTION('center_axis',(0.,1.,0.));
#11291=DIRECTION('ref_axis',(1.,0.,0.));
#11292=DIRECTION('center_axis',(0.,1.,0.));
#11293=DIRECTION('ref_axis',(1.,0.,0.));
#11294=DIRECTION('center_axis',(0.,1.,0.));
#11295=DIRECTION('ref_axis',(1.,0.,0.));
#11296=DIRECTION('center_axis',(0.,1.,0.));
#11297=DIRECTION('ref_axis',(1.,0.,0.));
#11298=DIRECTION('center_axis',(0.,1.,0.));
#11299=DIRECTION('ref_axis',(-1.,0.,-1.22464679914735E-16));
#11300=DIRECTION('center_axis',(0.,1.,0.));
#11301=DIRECTION('ref_axis',(1.,0.,0.));
#11302=DIRECTION('center_axis',(0.,1.,0.));
#11303=DIRECTION('ref_axis',(1.,0.,0.));
#11304=DIRECTION('',(0.,-1.,0.));
#11305=DIRECTION('center_axis',(0.,1.,0.));
#11306=DIRECTION('ref_axis',(1.,0.,0.));
#11307=DIRECTION('center_axis',(0.,1.,0.));
#11308=DIRECTION('ref_axis',(1.,0.,0.));
#11309=DIRECTION('center_axis',(0.,-1.,0.));
#11310=DIRECTION('ref_axis',(1.,0.,0.));
#11311=DIRECTION('center_axis',(0.,1.,0.));
#11312=DIRECTION('ref_axis',(1.,0.,0.));
#11313=DIRECTION('center_axis',(0.,-1.,0.));
#11314=DIRECTION('ref_axis',(1.,0.,0.));
#11315=DIRECTION('',(0.,-1.,0.));
#11316=DIRECTION('center_axis',(0.,1.,0.));
#11317=DIRECTION('ref_axis',(1.,0.,0.));
#11318=DIRECTION('axis',(0.,0.,1.));
#11319=DIRECTION('refdir',(1.,0.,0.));
#11320=DIRECTION('center_axis',(0.,1.,0.));
#11321=DIRECTION('ref_axis',(1.,0.,0.));
#11322=DIRECTION('center_axis',(0.,1.,0.));
#11323=DIRECTION('ref_axis',(1.,0.,0.));
#11324=DIRECTION('',(0.,1.,0.));
#11325=DIRECTION('center_axis',(0.,-1.,0.));
#11326=DIRECTION('ref_axis',(1.,0.,0.));
#11327=DIRECTION('center_axis',(0.,1.,0.));
#11328=DIRECTION('ref_axis',(1.,0.,0.));
#11329=DIRECTION('center_axis',(0.,1.,0.));
#11330=DIRECTION('ref_axis',(1.,0.,0.));
#11331=DIRECTION('',(0.,1.,0.));
#11332=DIRECTION('center_axis',(0.,-1.,0.));
#11333=DIRECTION('ref_axis',(1.,0.,0.));
#11334=DIRECTION('center_axis',(0.,1.,0.));
#11335=DIRECTION('ref_axis',(1.,0.,0.));
#11336=DIRECTION('center_axis',(0.,1.,0.));
#11337=DIRECTION('ref_axis',(1.,0.,0.));
#11338=DIRECTION('',(0.,1.,0.));
#11339=DIRECTION('center_axis',(0.,-1.,0.));
#11340=DIRECTION('ref_axis',(1.,0.,0.));
#11341=DIRECTION('center_axis',(0.,1.,0.));
#11342=DIRECTION('ref_axis',(1.,0.,0.));
#11343=DIRECTION('center_axis',(0.,1.,0.));
#11344=DIRECTION('ref_axis',(1.,0.,0.));
#11345=DIRECTION('',(0.,1.,0.));
#11346=DIRECTION('center_axis',(0.,-1.,0.));
#11347=DIRECTION('ref_axis',(1.,0.,0.));
#11348=DIRECTION('center_axis',(0.,1.,0.));
#11349=DIRECTION('ref_axis',(1.,0.,0.));
#11350=DIRECTION('center_axis',(0.,1.,0.));
#11351=DIRECTION('ref_axis',(1.,0.,0.));
#11352=DIRECTION('',(0.,1.,0.));
#11353=DIRECTION('center_axis',(0.,-1.,0.));
#11354=DIRECTION('ref_axis',(1.,0.,0.));
#11355=DIRECTION('center_axis',(0.,0.,1.));
#11356=DIRECTION('ref_axis',(1.,0.,0.));
#11357=DIRECTION('center_axis',(0.,0.,1.));
#11358=DIRECTION('ref_axis',(1.,0.,0.));
#11359=DIRECTION('',(0.,0.,1.));
#11360=DIRECTION('center_axis',(0.,0.,-1.));
#11361=DIRECTION('ref_axis',(1.,0.,0.));
#11362=DIRECTION('center_axis',(0.,0.,1.));
#11363=DIRECTION('ref_axis',(1.,0.,0.));
#11364=DIRECTION('center_axis',(0.,0.,1.));
#11365=DIRECTION('ref_axis',(1.,0.,0.));
#11366=DIRECTION('',(0.,0.,1.));
#11367=DIRECTION('center_axis',(0.,0.,-1.));
#11368=DIRECTION('ref_axis',(1.,0.,0.));
#11369=DIRECTION('center_axis',(0.,0.,1.));
#11370=DIRECTION('ref_axis',(1.,0.,0.));
#11371=DIRECTION('center_axis',(0.,0.,1.));
#11372=DIRECTION('ref_axis',(1.,0.,0.));
#11373=DIRECTION('',(0.,0.,1.));
#11374=DIRECTION('center_axis',(0.,0.,-1.));
#11375=DIRECTION('ref_axis',(1.,0.,0.));
#11376=DIRECTION('center_axis',(0.,0.,1.));
#11377=DIRECTION('ref_axis',(1.,0.,0.));
#11378=DIRECTION('center_axis',(0.,0.,1.));
#11379=DIRECTION('ref_axis',(1.,0.,0.));
#11380=DIRECTION('',(0.,0.,1.));
#11381=DIRECTION('center_axis',(0.,0.,-1.));
#11382=DIRECTION('ref_axis',(1.,0.,0.));
#11383=DIRECTION('center_axis',(0.,0.,1.));
#11384=DIRECTION('ref_axis',(1.,0.,0.));
#11385=DIRECTION('',(0.,1.,0.));
#11386=DIRECTION('',(-1.,0.,0.));
#11387=DIRECTION('',(0.,1.,0.));
#11388=DIRECTION('',(1.,0.,0.));
#11389=DIRECTION('center_axis',(0.,0.,1.));
#11390=DIRECTION('ref_axis',(1.,0.,0.));
#11391=DIRECTION('',(0.,-1.,0.));
#11392=DIRECTION('',(1.,0.,0.));
#11393=DIRECTION('',(0.,1.,0.));
#11394=DIRECTION('',(-1.,0.,0.));
#11395=DIRECTION('center_axis',(-1.,0.,0.));
#11396=DIRECTION('ref_axis',(0.,0.,1.));
#11397=DIRECTION('',(0.,0.,-1.));
#11398=DIRECTION('',(0.,0.,1.));
#11399=DIRECTION('',(0.,1.,0.));
#11400=DIRECTION('center_axis',(1.,0.,0.));
#11401=DIRECTION('ref_axis',(0.,0.,-1.));
#11402=DIRECTION('',(0.,0.,1.));
#11403=DIRECTION('',(0.,1.,0.));
#11404=DIRECTION('',(0.,0.,-1.));
#11405=DIRECTION('center_axis',(0.,-1.,0.));
#11406=DIRECTION('ref_axis',(1.,0.,0.));
#11407=DIRECTION('',(0.,0.,1.));
#11408=DIRECTION('',(1.,0.,0.));
#11409=DIRECTION('',(0.,0.,1.));
#11410=DIRECTION('',(1.,0.,0.));
#11411=DIRECTION('center_axis',(1.,0.,0.));
#11412=DIRECTION('ref_axis',(0.,1.,0.));
#11413=DIRECTION('',(0.,0.,1.));
#11414=DIRECTION('',(0.,1.,0.));
#11415=DIRECTION('center_axis',(0.,1.,0.));
#11416=DIRECTION('ref_axis',(-1.,0.,0.));
#11417=DIRECTION('',(0.,0.,1.));
#11418=DIRECTION('',(-1.,0.,0.));
#11419=DIRECTION('',(-1.,0.,0.));
#11420=DIRECTION('center_axis',(-1.,0.,0.));
#11421=DIRECTION('ref_axis',(0.,-1.,0.));
#11422=DIRECTION('',(0.,-1.,0.));
#11423=DIRECTION('center_axis',(0.,0.,1.));
#11424=DIRECTION('ref_axis',(1.,0.,0.));
#11425=DIRECTION('center_axis',(0.,0.,1.));
#11426=DIRECTION('ref_axis',(1.,0.,0.));
#11427=DIRECTION('axis',(0.,0.,1.));
#11428=DIRECTION('refdir',(1.,0.,0.));
#11429=DIRECTION('center_axis',(0.,0.,1.));
#11430=DIRECTION('ref_axis',(1.,0.,0.));
#11431=DIRECTION('center_axis',(0.,0.,-1.));
#11432=DIRECTION('ref_axis',(1.,0.,0.));
#11433=DIRECTION('',(0.,0.,-1.));
#11434=DIRECTION('center_axis',(0.,0.,-1.));
#11435=DIRECTION('ref_axis',(1.,0.,0.));
#11436=DIRECTION('center_axis',(0.,0.,1.));
#11437=DIRECTION('ref_axis',(1.,0.,0.));
#11438=DIRECTION('center_axis',(0.,0.,1.));
#11439=DIRECTION('ref_axis',(1.,0.,0.));
#11440=DIRECTION('',(0.,0.,-1.));
#11441=DIRECTION('center_axis',(0.,0.,1.));
#11442=DIRECTION('ref_axis',(1.,0.,0.));
#11443=DIRECTION('center_axis',(0.,0.,1.));
#11444=DIRECTION('ref_axis',(1.,0.,0.));
#11445=DIRECTION('center_axis',(0.,0.,1.));
#11446=DIRECTION('ref_axis',(1.,0.,0.));
#11447=DIRECTION('axis',(0.,0.,1.));
#11448=DIRECTION('refdir',(1.,0.,0.));
#11449=DIRECTION('center_axis',(0.,0.,1.));
#11450=DIRECTION('ref_axis',(1.,0.,0.));
#11451=DIRECTION('center_axis',(0.,0.,-1.));
#11452=DIRECTION('ref_axis',(1.,0.,0.));
#11453=DIRECTION('',(0.,0.,-1.));
#11454=DIRECTION('center_axis',(0.,0.,-1.));
#11455=DIRECTION('ref_axis',(1.,0.,0.));
#11456=DIRECTION('center_axis',(0.,0.,1.));
#11457=DIRECTION('ref_axis',(1.,0.,0.));
#11458=DIRECTION('center_axis',(0.,0.,1.));
#11459=DIRECTION('ref_axis',(1.,0.,0.));
#11460=DIRECTION('',(0.,0.,-1.));
#11461=DIRECTION('center_axis',(0.,0.,1.));
#11462=DIRECTION('ref_axis',(1.,0.,0.));
#11463=DIRECTION('center_axis',(0.,0.,1.));
#11464=DIRECTION('ref_axis',(1.,0.,0.));
#11465=DIRECTION('center_axis',(0.,0.,1.));
#11466=DIRECTION('ref_axis',(1.,0.,0.));
#11467=DIRECTION('axis',(0.,0.,1.));
#11468=DIRECTION('refdir',(1.,0.,0.));
#11469=DIRECTION('center_axis',(0.,0.,1.));
#11470=DIRECTION('ref_axis',(1.,0.,0.));
#11471=DIRECTION('center_axis',(0.,0.,-1.));
#11472=DIRECTION('ref_axis',(1.,0.,0.));
#11473=DIRECTION('',(0.,0.,-1.));
#11474=DIRECTION('center_axis',(0.,0.,-1.));
#11475=DIRECTION('ref_axis',(1.,0.,0.));
#11476=DIRECTION('center_axis',(0.,0.,1.));
#11477=DIRECTION('ref_axis',(1.,0.,0.));
#11478=DIRECTION('center_axis',(0.,0.,1.));
#11479=DIRECTION('ref_axis',(1.,0.,0.));
#11480=DIRECTION('',(0.,0.,-1.));
#11481=DIRECTION('center_axis',(0.,0.,1.));
#11482=DIRECTION('ref_axis',(1.,0.,0.));
#11483=DIRECTION('center_axis',(0.,0.,1.));
#11484=DIRECTION('ref_axis',(1.,0.,0.));
#11485=DIRECTION('center_axis',(0.,0.,1.));
#11486=DIRECTION('ref_axis',(1.,0.,0.));
#11487=DIRECTION('axis',(0.,0.,1.));
#11488=DIRECTION('refdir',(1.,0.,0.));
#11489=DIRECTION('center_axis',(0.,0.,1.));
#11490=DIRECTION('ref_axis',(1.,0.,0.));
#11491=DIRECTION('center_axis',(0.,0.,-1.));
#11492=DIRECTION('ref_axis',(1.,0.,0.));
#11493=DIRECTION('',(0.,0.,-1.));
#11494=DIRECTION('center_axis',(0.,0.,-1.));
#11495=DIRECTION('ref_axis',(1.,0.,0.));
#11496=DIRECTION('center_axis',(0.,0.,1.));
#11497=DIRECTION('ref_axis',(1.,0.,0.));
#11498=DIRECTION('center_axis',(0.,0.,1.));
#11499=DIRECTION('ref_axis',(1.,0.,0.));
#11500=DIRECTION('',(0.,0.,-1.));
#11501=DIRECTION('center_axis',(0.,0.,1.));
#11502=DIRECTION('ref_axis',(1.,0.,0.));
#11503=DIRECTION('center_axis',(0.,0.,1.));
#11504=DIRECTION('ref_axis',(1.,0.,0.));
#11505=DIRECTION('center_axis',(0.,0.,1.));
#11506=DIRECTION('ref_axis',(1.,0.,0.));
#11507=DIRECTION('axis',(0.,0.,1.));
#11508=DIRECTION('refdir',(1.,0.,0.));
#11509=DIRECTION('center_axis',(0.,1.,0.));
#11510=DIRECTION('ref_axis',(1.,0.,0.));
#11511=DIRECTION('center_axis',(0.,-1.,0.));
#11512=DIRECTION('ref_axis',(1.,0.,0.));
#11513=DIRECTION('',(0.,-1.,0.));
#11514=DIRECTION('center_axis',(0.,-1.,0.));
#11515=DIRECTION('ref_axis',(1.,0.,0.));
#11516=DIRECTION('center_axis',(0.,1.,0.));
#11517=DIRECTION('ref_axis',(1.,0.,0.));
#11518=DIRECTION('center_axis',(0.,1.,0.));
#11519=DIRECTION('ref_axis',(1.,0.,0.));
#11520=DIRECTION('',(0.,-1.,0.));
#11521=DIRECTION('center_axis',(0.,1.,0.));
#11522=DIRECTION('ref_axis',(1.,0.,0.));
#11523=DIRECTION('center_axis',(0.,1.,0.));
#11524=DIRECTION('ref_axis',(1.,0.,0.));
#11525=DIRECTION('center_axis',(0.,1.,0.));
#11526=DIRECTION('ref_axis',(1.,0.,0.));
#11527=DIRECTION('axis',(0.,0.,1.));
#11528=DIRECTION('refdir',(1.,0.,0.));
#11529=DIRECTION('center_axis',(0.,1.,0.));
#11530=DIRECTION('ref_axis',(0.707106781186546,0.,0.707106781186549));
#11531=DIRECTION('',(0.,1.,0.));
#11532=DIRECTION('center_axis',(0.,1.,0.));
#11533=DIRECTION('ref_axis',(1.,0.,0.));
#11534=DIRECTION('',(0.,-1.,0.));
#11535=DIRECTION('center_axis',(0.,-1.,0.));
#11536=DIRECTION('ref_axis',(1.,0.,0.));
#11537=DIRECTION('center_axis',(0.,1.,0.));
#11538=DIRECTION('ref_axis',(0.707106781186544,0.,-0.707106781186551));
#11539=DIRECTION('',(0.,1.,0.));
#11540=DIRECTION('center_axis',(0.,1.,0.));
#11541=DIRECTION('ref_axis',(1.,0.,0.));
#11542=DIRECTION('',(0.,-1.,0.));
#11543=DIRECTION('center_axis',(0.,-1.,0.));
#11544=DIRECTION('ref_axis',(1.,0.,0.));
#11545=DIRECTION('center_axis',(0.,1.,0.));
#11546=DIRECTION('ref_axis',(-0.707106781186548,0.,-0.707106781186547));
#11547=DIRECTION('',(0.,1.,0.));
#11548=DIRECTION('center_axis',(0.,1.,0.));
#11549=DIRECTION('ref_axis',(1.,0.,0.));
#11550=DIRECTION('',(0.,-1.,0.));
#11551=DIRECTION('center_axis',(0.,-1.,0.));
#11552=DIRECTION('ref_axis',(1.,0.,0.));
#11553=DIRECTION('center_axis',(0.,1.,0.));
#11554=DIRECTION('ref_axis',(-0.707106781186544,0.,0.707106781186551));
#11555=DIRECTION('',(0.,1.,0.));
#11556=DIRECTION('center_axis',(0.,1.,0.));
#11557=DIRECTION('ref_axis',(1.,0.,0.));
#11558=DIRECTION('',(0.,-1.,0.));
#11559=DIRECTION('center_axis',(0.,-1.,0.));
#11560=DIRECTION('ref_axis',(1.,0.,0.));
#11561=DIRECTION('center_axis',(0.,1.,0.));
#11562=DIRECTION('ref_axis',(1.,0.,0.));
#11563=DIRECTION('center_axis',(0.,1.,0.));
#11564=DIRECTION('ref_axis',(1.,0.,0.));
#11565=DIRECTION('center_axis',(0.,1.,0.));
#11566=DIRECTION('ref_axis',(1.,0.,0.));
#11567=DIRECTION('center_axis',(0.,1.,0.));
#11568=DIRECTION('ref_axis',(1.,0.,0.));
#11569=DIRECTION('center_axis',(0.,1.,0.));
#11570=DIRECTION('ref_axis',(1.,0.,0.));
#11571=DIRECTION('center_axis',(0.,-1.,0.));
#11572=DIRECTION('ref_axis',(1.,0.,0.));
#11573=DIRECTION('center_axis',(0.,1.,0.));
#11574=DIRECTION('ref_axis',(1.,0.,0.));
#11575=DIRECTION('center_axis',(0.,1.,0.));
#11576=DIRECTION('ref_axis',(1.,0.,0.));
#11577=DIRECTION('center_axis',(0.,1.,0.));
#11578=DIRECTION('ref_axis',(1.,0.,0.));
#11579=DIRECTION('center_axis',(0.,1.,0.));
#11580=DIRECTION('ref_axis',(1.,0.,0.));
#11581=DIRECTION('center_axis',(0.,1.,0.));
#11582=DIRECTION('ref_axis',(1.,0.,0.));
#11583=DIRECTION('center_axis',(0.,1.,0.));
#11584=DIRECTION('ref_axis',(1.,0.,0.));
#11585=DIRECTION('center_axis',(0.,1.,0.));
#11586=DIRECTION('ref_axis',(-1.,0.,-1.01064309961486E-15));
#11587=DIRECTION('center_axis',(0.,1.,0.));
#11588=DIRECTION('ref_axis',(1.,0.,0.));
#11589=DIRECTION('center_axis',(0.,1.,0.));
#11590=DIRECTION('ref_axis',(1.,0.,0.));
#11591=DIRECTION('center_axis',(0.,1.,0.));
#11592=DIRECTION('ref_axis',(1.,0.,0.));
#11593=DIRECTION('',(0.,-1.,0.));
#11594=DIRECTION('center_axis',(0.,-1.,0.));
#11595=DIRECTION('ref_axis',(1.,0.,0.));
#11596=DIRECTION('center_axis',(0.,1.,0.));
#11597=DIRECTION('ref_axis',(1.,0.,0.));
#11598=DIRECTION('center_axis',(0.,-1.,0.));
#11599=DIRECTION('ref_axis',(1.,0.,0.));
#11600=DIRECTION('center_axis',(0.,1.,0.));
#11601=DIRECTION('ref_axis',(1.,0.,0.));
#11602=DIRECTION('',(0.,-1.,0.));
#11603=DIRECTION('center_axis',(0.,1.,0.));
#11604=DIRECTION('ref_axis',(1.,0.,0.));
#11605=DIRECTION('axis',(0.,0.,1.));
#11606=DIRECTION('refdir',(1.,0.,0.));
#11607=DIRECTION('center_axis',(0.,1.,0.));
#11608=DIRECTION('ref_axis',(0.707106781186546,0.,0.707106781186549));
#11609=DIRECTION('',(0.,1.,0.));
#11610=DIRECTION('center_axis',(0.,1.,0.));
#11611=DIRECTION('ref_axis',(1.,0.,0.));
#11612=DIRECTION('',(0.,-1.,0.));
#11613=DIRECTION('center_axis',(0.,-1.,0.));
#11614=DIRECTION('ref_axis',(1.,0.,0.));
#11615=DIRECTION('center_axis',(0.,1.,0.));
#11616=DIRECTION('ref_axis',(0.707106781186544,0.,-0.707106781186551));
#11617=DIRECTION('',(0.,1.,0.));
#11618=DIRECTION('center_axis',(0.,1.,0.));
#11619=DIRECTION('ref_axis',(1.,0.,0.));
#11620=DIRECTION('',(0.,-1.,0.));
#11621=DIRECTION('center_axis',(0.,-1.,0.));
#11622=DIRECTION('ref_axis',(1.,0.,0.));
#11623=DIRECTION('center_axis',(0.,1.,0.));
#11624=DIRECTION('ref_axis',(-0.707106781186548,0.,-0.707106781186547));
#11625=DIRECTION('',(0.,1.,0.));
#11626=DIRECTION('center_axis',(0.,1.,0.));
#11627=DIRECTION('ref_axis',(1.,0.,0.));
#11628=DIRECTION('',(0.,-1.,0.));
#11629=DIRECTION('center_axis',(0.,-1.,0.));
#11630=DIRECTION('ref_axis',(1.,0.,0.));
#11631=DIRECTION('center_axis',(0.,1.,0.));
#11632=DIRECTION('ref_axis',(-0.707106781186544,0.,0.707106781186551));
#11633=DIRECTION('',(0.,1.,0.));
#11634=DIRECTION('center_axis',(0.,1.,0.));
#11635=DIRECTION('ref_axis',(1.,0.,0.));
#11636=DIRECTION('',(0.,-1.,0.));
#11637=DIRECTION('center_axis',(0.,-1.,0.));
#11638=DIRECTION('ref_axis',(1.,0.,0.));
#11639=DIRECTION('center_axis',(0.,1.,0.));
#11640=DIRECTION('ref_axis',(1.,0.,0.));
#11641=DIRECTION('center_axis',(0.,1.,0.));
#11642=DIRECTION('ref_axis',(1.,0.,0.));
#11643=DIRECTION('center_axis',(0.,1.,0.));
#11644=DIRECTION('ref_axis',(1.,0.,0.));
#11645=DIRECTION('center_axis',(0.,1.,0.));
#11646=DIRECTION('ref_axis',(1.,0.,0.));
#11647=DIRECTION('center_axis',(0.,1.,0.));
#11648=DIRECTION('ref_axis',(1.,0.,0.));
#11649=DIRECTION('center_axis',(0.,1.,0.));
#11650=DIRECTION('ref_axis',(1.,0.,0.));
#11651=DIRECTION('center_axis',(0.,1.,0.));
#11652=DIRECTION('ref_axis',(1.,0.,0.));
#11653=DIRECTION('center_axis',(0.,1.,0.));
#11654=DIRECTION('ref_axis',(1.,0.,0.));
#11655=DIRECTION('center_axis',(0.,1.,0.));
#11656=DIRECTION('ref_axis',(1.,0.,0.));
#11657=DIRECTION('center_axis',(0.,1.,0.));
#11658=DIRECTION('ref_axis',(1.,0.,0.));
#11659=DIRECTION('center_axis',(0.,1.,0.));
#11660=DIRECTION('ref_axis',(1.,0.,0.));
#11661=DIRECTION('center_axis',(0.,1.,0.));
#11662=DIRECTION('ref_axis',(1.,0.,0.));
#11663=DIRECTION('center_axis',(0.,1.,0.));
#11664=DIRECTION('ref_axis',(-1.,0.,-1.01064309961486E-15));
#11665=DIRECTION('center_axis',(0.,1.,0.));
#11666=DIRECTION('ref_axis',(1.,0.,0.));
#11667=DIRECTION('center_axis',(0.,1.,0.));
#11668=DIRECTION('ref_axis',(1.,0.,0.));
#11669=DIRECTION('',(0.,-1.,0.));
#11670=DIRECTION('center_axis',(0.,1.,0.));
#11671=DIRECTION('ref_axis',(1.,0.,0.));
#11672=DIRECTION('center_axis',(0.,1.,0.));
#11673=DIRECTION('ref_axis',(1.,0.,0.));
#11674=DIRECTION('center_axis',(0.,-1.,0.));
#11675=DIRECTION('ref_axis',(1.,0.,0.));
#11676=DIRECTION('center_axis',(0.,1.,0.));
#11677=DIRECTION('ref_axis',(1.,0.,0.));
#11678=DIRECTION('center_axis',(0.,-1.,0.));
#11679=DIRECTION('ref_axis',(1.,0.,0.));
#11680=DIRECTION('',(0.,-1.,0.));
#11681=DIRECTION('center_axis',(0.,1.,0.));
#11682=DIRECTION('ref_axis',(1.,0.,0.));
#11683=DIRECTION('axis',(0.,0.,1.));
#11684=DIRECTION('refdir',(1.,0.,0.));
#11685=DIRECTION('center_axis',(-0.0913252028230577,0.,-0.99582112215464));
#11686=DIRECTION('ref_axis',(-0.99582112215464,0.,0.0913252028230577));
#11687=DIRECTION('',(-0.99582112215464,0.,0.0913252028230577));
#11688=DIRECTION('',(0.,-1.,0.));
#11689=DIRECTION('',(0.99582112215464,0.,-0.0913252028230577));
#11690=DIRECTION('',(0.,-1.,0.));
#11691=DIRECTION('center_axis',(-0.0913252028230577,0.,0.99582112215464));
#11692=DIRECTION('ref_axis',(0.99582112215464,0.,0.0913252028230577));
#11693=DIRECTION('',(0.99582112215464,0.,0.0913252028230577));
#11694=DIRECTION('',(0.,-1.,0.));
#11695=DIRECTION('',(-0.99582112215464,0.,-0.0913252028230577));
#11696=DIRECTION('',(0.,1.,0.));
#11697=DIRECTION('center_axis',(0.,1.,0.));
#11698=DIRECTION('ref_axis',(1.,0.,0.));
#11699=DIRECTION('',(0.99582112215464,0.,0.091325202823058));
#11700=DIRECTION('center_axis',(0.,1.,0.));
#11701=DIRECTION('ref_axis',(1.,0.,0.));
#11702=DIRECTION('',(-0.99582112215464,0.,0.0913252028230577));
#11703=DIRECTION('center_axis',(0.,1.,0.));
#11704=DIRECTION('ref_axis',(1.,0.,0.));
#11705=DIRECTION('center_axis',(0.,1.,0.));
#11706=DIRECTION('ref_axis',(1.,0.,0.));
#11707=DIRECTION('center_axis',(0.,1.,0.));
#11708=DIRECTION('ref_axis',(1.,0.,0.));
#11709=DIRECTION('center_axis',(0.,1.,0.));
#11710=DIRECTION('ref_axis',(-1.,0.,-1.22464679914735E-16));
#11711=DIRECTION('center_axis',(0.,-1.,0.));
#11712=DIRECTION('ref_axis',(1.,0.,0.));
#11713=DIRECTION('center_axis',(0.,1.,0.));
#11714=DIRECTION('ref_axis',(1.,0.,0.));
#11715=DIRECTION('center_axis',(0.,-1.,0.));
#11716=DIRECTION('ref_axis',(1.,0.,0.));
#11717=DIRECTION('center_axis',(0.,1.,0.));
#11718=DIRECTION('ref_axis',(1.,0.,0.));
#11719=DIRECTION('',(0.,1.,0.));
#11720=DIRECTION('center_axis',(0.,1.,0.));
#11721=DIRECTION('ref_axis',(1.,0.,0.));
#11722=DIRECTION('',(0.,1.,0.));
#11723=DIRECTION('center_axis',(-0.0913252028230577,0.,-0.99582112215464));
#11724=DIRECTION('ref_axis',(-0.99582112215464,0.,0.0913252028230577));
#11725=DIRECTION('',(0.,1.,0.));
#11726=DIRECTION('',(-0.99582112215464,0.,0.0913252028230577));
#11727=DIRECTION('center_axis',(-0.091325202823058,0.,0.99582112215464));
#11728=DIRECTION('ref_axis',(0.99582112215464,0.,0.091325202823058));
#11729=DIRECTION('',(0.99582112215464,0.,0.091325202823058));
#11730=DIRECTION('',(0.,1.,0.));
#11731=DIRECTION('center_axis',(0.,1.,0.));
#11732=DIRECTION('ref_axis',(-1.,0.,-1.22464679914735E-16));
#11733=DIRECTION('center_axis',(0.,1.,0.));
#11734=DIRECTION('ref_axis',(1.,0.,0.));
#11735=DIRECTION('center_axis',(0.,1.,0.));
#11736=DIRECTION('ref_axis',(1.,0.,0.));
#11737=DIRECTION('axis',(0.,0.,1.));
#11738=DIRECTION('refdir',(1.,0.,0.));
#11739=DIRECTION('axis',(0.,0.,1.));
#11740=DIRECTION('refdir',(1.,0.,0.));
#11741=DIRECTION('center_axis',(0.,-1.,0.));
#11742=DIRECTION('ref_axis',(0.,0.,-1.));
#11743=DIRECTION('center_axis',(0.,-1.,0.));
#11744=DIRECTION('ref_axis',(1.,0.,0.));
#11745=DIRECTION('center_axis',(0.,-1.,0.));
#11746=DIRECTION('ref_axis',(1.,0.,0.));
#11747=DIRECTION('center_axis',(1.,0.,1.22464679914735E-16));
#11748=DIRECTION('ref_axis',(-1.22464679914735E-16,0.,1.));
#11749=DIRECTION('center_axis',(0.,1.,0.));
#11750=DIRECTION('ref_axis',(1.,0.,0.));
#11751=DIRECTION('center_axis',(0.,1.,0.));
#11752=DIRECTION('ref_axis',(1.,0.,0.));
#11753=DIRECTION('center_axis',(0.,-1.,0.));
#11754=DIRECTION('ref_axis',(1.,0.,0.));
#11755=DIRECTION('',(0.,1.,0.));
#11756=DIRECTION('center_axis',(0.,-1.,0.));
#11757=DIRECTION('ref_axis',(1.,0.,0.));
#11758=DIRECTION('center_axis',(0.,-1.,0.));
#11759=DIRECTION('ref_axis',(1.,0.,0.));
#11760=DIRECTION('center_axis',(0.,-1.,0.));
#11761=DIRECTION('ref_axis',(1.,0.,0.));
#11762=DIRECTION('',(0.,1.,0.));
#11763=DIRECTION('center_axis',(0.,-1.,0.));
#11764=DIRECTION('ref_axis',(1.,0.,0.));
#11765=DIRECTION('center_axis',(0.,1.,0.));
#11766=DIRECTION('ref_axis',(1.,0.,0.));
#11767=DIRECTION('',(-0.707106781186547,0.707106781186548,-8.65956056235493E-17));
#11768=DIRECTION('center_axis',(0.,-1.,0.));
#11769=DIRECTION('ref_axis',(1.,0.,0.));
#11770=DIRECTION('center_axis',(0.,1.,0.));
#11771=DIRECTION('ref_axis',(0.,0.,1.));
#11772=DIRECTION('center_axis',(0.,-1.,0.));
#11773=DIRECTION('ref_axis',(1.,0.,0.));
#11774=DIRECTION('center_axis',(0.,-1.,0.));
#11775=DIRECTION('ref_axis',(1.,0.,0.));
#11776=DIRECTION('',(0.,1.,0.));
#11777=DIRECTION('center_axis',(0.,-1.,0.));
#11778=DIRECTION('ref_axis',(0.,0.,-1.));
#11779=DIRECTION('center_axis',(0.,-1.,0.));
#11780=DIRECTION('ref_axis',(1.,0.,0.));
#11781=DIRECTION('center_axis',(0.,-1.,0.));
#11782=DIRECTION('ref_axis',(1.,0.,0.));
#11783=DIRECTION('',(0.707106781186547,0.707106781186548,8.65956056235493E-17));
#11784=DIRECTION('axis',(0.,0.,1.));
#11785=DIRECTION('refdir',(1.,0.,0.));
#11786=DIRECTION('center_axis',(0.,-1.,0.));
#11787=DIRECTION('ref_axis',(0.,0.,-1.));
#11788=DIRECTION('center_axis',(0.,-1.,0.));
#11789=DIRECTION('ref_axis',(1.,0.,0.));
#11790=DIRECTION('center_axis',(0.,-1.,0.));
#11791=DIRECTION('ref_axis',(1.,0.,0.));
#11792=DIRECTION('center_axis',(1.,0.,1.22464679914735E-16));
#11793=DIRECTION('ref_axis',(-1.22464679914735E-16,0.,1.));
#11794=DIRECTION('center_axis',(0.,1.,0.));
#11795=DIRECTION('ref_axis',(1.,0.,0.));
#11796=DIRECTION('center_axis',(0.,1.,0.));
#11797=DIRECTION('ref_axis',(1.,0.,0.));
#11798=DIRECTION('center_axis',(0.,-1.,0.));
#11799=DIRECTION('ref_axis',(1.,0.,0.));
#11800=DIRECTION('center_axis',(0.,-1.,0.));
#11801=DIRECTION('ref_axis',(1.,0.,0.));
#11802=DIRECTION('',(0.,1.,0.));
#11803=DIRECTION('center_axis',(0.,1.,0.));
#11804=DIRECTION('ref_axis',(0.,0.,1.));
#11805=DIRECTION('center_axis',(0.,-1.,0.));
#11806=DIRECTION('ref_axis',(1.,0.,0.));
#11807=DIRECTION('center_axis',(0.,-1.,0.));
#11808=DIRECTION('ref_axis',(1.,0.,0.));
#11809=DIRECTION('center_axis',(0.,-1.,0.));
#11810=DIRECTION('ref_axis',(1.,0.,0.));
#11811=DIRECTION('center_axis',(0.,-1.,0.));
#11812=DIRECTION('ref_axis',(1.,0.,0.));
#11813=DIRECTION('',(0.707106781186548,0.707106781186547,8.65956056235494E-17));
#11814=DIRECTION('center_axis',(0.,-1.,0.));
#11815=DIRECTION('ref_axis',(1.,0.,0.));
#11816=DIRECTION('center_axis',(0.,-1.,0.));
#11817=DIRECTION('ref_axis',(1.,0.,0.));
#11818=DIRECTION('',(0.,1.,0.));
#11819=DIRECTION('center_axis',(0.,1.,0.));
#11820=DIRECTION('ref_axis',(1.,0.,0.));
#11821=DIRECTION('center_axis',(0.,-1.,0.));
#11822=DIRECTION('ref_axis',(1.,0.,0.));
#11823=DIRECTION('',(-0.707106781186548,0.707106781186547,-8.65956056235494E-17));
#11824=DIRECTION('center_axis',(0.,-1.,0.));
#11825=DIRECTION('ref_axis',(0.,0.,-1.));
#11826=DIRECTION('center_axis',(0.,-1.,0.));
#11827=DIRECTION('ref_axis',(1.,0.,0.));
#11828=DIRECTION('',(0.,1.,0.));
#11829=DIRECTION('axis',(0.,0.,1.));
#11830=DIRECTION('refdir',(1.,0.,0.));
#11831=DIRECTION('center_axis',(0.,0.,1.));
#11832=DIRECTION('ref_axis',(1.,0.,0.));
#11833=DIRECTION('center_axis',(1.22464679914735E-16,-1.,0.));
#11834=DIRECTION('ref_axis',(-1.,-1.22464679914735E-16,0.));
#11835=DIRECTION('center_axis',(0.707106781186548,0.,0.707106781186548));
#11836=DIRECTION('ref_axis',(0.707106781186548,0.,-0.707106781186548));
#11837=DIRECTION('center_axis',(8.65956056235494E-17,-1.,-8.65956056235493E-17));
#11838=DIRECTION('ref_axis',(-0.707106781186547,-1.22464679914735E-16,0.707106781186547));
#11839=DIRECTION('center_axis',(1.,0.,0.));
#11840=DIRECTION('ref_axis',(6.12323399573676E-17,0.,-1.));
#11841=DIRECTION('center_axis',(7.49879891330929E-33,-1.,-1.22464679914735E-16));
#11842=DIRECTION('ref_axis',(-6.12323399573676E-17,-1.22464679914735E-16,
1.));
#11843=DIRECTION('center_axis',(0.707106781186548,0.,-0.707106781186548));
#11844=DIRECTION('ref_axis',(-0.707106781186548,0.,-0.707106781186548));
#11845=DIRECTION('center_axis',(-8.65956056235493E-17,-1.,-8.65956056235494E-17));
#11846=DIRECTION('ref_axis',(0.707106781186547,-1.22464679914735E-16,0.707106781186547));
#11847=DIRECTION('center_axis',(0.,0.,-1.));
#11848=DIRECTION('ref_axis',(-1.,0.,-1.22464679914735E-16));
#11849=DIRECTION('center_axis',(-1.22464679914735E-16,-1.,-1.49975978266186E-32));
#11850=DIRECTION('ref_axis',(1.,-1.22464679914735E-16,1.22464679914735E-16));
#11851=DIRECTION('center_axis',(-0.707106781186547,0.,-0.707106781186548));
#11852=DIRECTION('ref_axis',(-0.707106781186548,0.,0.707106781186547));
#11853=DIRECTION('center_axis',(-8.65956056235493E-17,-1.,8.65956056235493E-17));
#11854=DIRECTION('ref_axis',(0.707106781186548,-1.22464679914735E-16,-0.707106781186547));
#11855=DIRECTION('center_axis',(-1.,0.,0.));
#11856=DIRECTION('ref_axis',(-1.83697019872103E-16,0.,1.));
#11857=DIRECTION('center_axis',(-2.24963967399279E-32,-1.,1.22464679914735E-16));
#11858=DIRECTION('ref_axis',(1.83697019872103E-16,-1.22464679914735E-16,
-1.));
#11859=DIRECTION('center_axis',(-0.707106781186548,0.,0.707106781186548));
#11860=DIRECTION('ref_axis',(0.707106781186547,0.,0.707106781186548));
#11861=DIRECTION('center_axis',(8.65956056235493E-17,-1.,8.65956056235493E-17));
#11862=DIRECTION('ref_axis',(-0.707106781186547,-1.22464679914735E-16,-0.707106781186548));
#11863=DIRECTION('axis',(0.,0.,1.));
#11864=DIRECTION('refdir',(1.,0.,0.));
#11865=DIRECTION('center_axis',(0.,0.,1.));
#11866=DIRECTION('ref_axis',(1.,0.,0.));
#11867=DIRECTION('center_axis',(0.,-1.,0.));
#11868=DIRECTION('ref_axis',(0.,0.,-1.));
#11869=DIRECTION('center_axis',(0.,-1.,0.));
#11870=DIRECTION('ref_axis',(0.,0.,-1.));
#11871=DIRECTION('center_axis',(0.,1.,0.));
#11872=DIRECTION('ref_axis',(1.,0.,0.));
#11873=DIRECTION('center_axis',(0.,1.,0.));
#11874=DIRECTION('ref_axis',(1.,0.,0.));
#11875=DIRECTION('center_axis',(0.,1.,0.));
#11876=DIRECTION('ref_axis',(1.,0.,0.));
#11877=DIRECTION('center_axis',(0.,1.,0.));
#11878=DIRECTION('ref_axis',(1.,0.,0.));
#11879=DIRECTION('',(0.,-1.,0.));
#11880=DIRECTION('center_axis',(0.,-1.,0.));
#11881=DIRECTION('ref_axis',(1.,0.,0.));
#11882=DIRECTION('center_axis',(0.,1.,0.));
#11883=DIRECTION('ref_axis',(1.,0.,0.));
#11884=DIRECTION('center_axis',(0.,1.,0.));
#11885=DIRECTION('ref_axis',(1.,0.,0.));
#11886=DIRECTION('center_axis',(0.,1.,0.));
#11887=DIRECTION('ref_axis',(1.,0.,0.));
#11888=DIRECTION('center_axis',(0.,1.,0.));
#11889=DIRECTION('ref_axis',(1.,0.,0.));
#11890=DIRECTION('center_axis',(0.,1.,0.));
#11891=DIRECTION('ref_axis',(1.,0.,0.));
#11892=DIRECTION('center_axis',(0.,1.,0.));
#11893=DIRECTION('ref_axis',(1.,0.,0.));
#11894=DIRECTION('center_axis',(0.,-1.,0.));
#11895=DIRECTION('ref_axis',(1.,0.,0.));
#11896=DIRECTION('center_axis',(0.,-1.,0.));
#11897=DIRECTION('ref_axis',(0.,0.,-1.));
#11898=DIRECTION('center_axis',(6.12323399573677E-17,0.,1.));
#11899=DIRECTION('ref_axis',(1.,0.,0.));
#11900=DIRECTION('center_axis',(0.,-1.,0.));
#11901=DIRECTION('ref_axis',(0.,0.,-1.));
#11902=DIRECTION('center_axis',(0.,1.,0.));
#11903=DIRECTION('ref_axis',(1.,0.,0.));
#11904=DIRECTION('center_axis',(0.,-1.,0.));
#11905=DIRECTION('ref_axis',(1.,0.,0.));
#11906=DIRECTION('center_axis',(0.,-1.,0.));
#11907=DIRECTION('ref_axis',(0.,0.,-1.));
#11908=DIRECTION('center_axis',(0.,0.,1.));
#11909=DIRECTION('ref_axis',(1.,0.,0.));
#11910=DIRECTION('center_axis',(0.,-1.,0.));
#11911=DIRECTION('ref_axis',(0.,0.,-1.));
#11912=DIRECTION('center_axis',(0.,1.,0.));
#11913=DIRECTION('ref_axis',(1.,0.,0.));
#11914=DIRECTION('center_axis',(0.,-1.,0.));
#11915=DIRECTION('ref_axis',(1.,0.,0.));
#11916=DIRECTION('center_axis',(0.,-1.,0.));
#11917=DIRECTION('ref_axis',(0.,0.,-1.));
#11918=DIRECTION('center_axis',(0.,0.,1.));
#11919=DIRECTION('ref_axis',(1.,0.,0.));
#11920=DIRECTION('center_axis',(0.,-1.,0.));
#11921=DIRECTION('ref_axis',(0.,0.,-1.));
#11922=DIRECTION('center_axis',(0.,1.,0.));
#11923=DIRECTION('ref_axis',(1.,0.,0.));
#11924=DIRECTION('center_axis',(0.,-1.,0.));
#11925=DIRECTION('ref_axis',(1.,0.,0.));
#11926=DIRECTION('center_axis',(0.,-1.,0.));
#11927=DIRECTION('ref_axis',(0.,0.,-1.));
#11928=DIRECTION('center_axis',(0.,0.,1.));
#11929=DIRECTION('ref_axis',(1.,0.,0.));
#11930=DIRECTION('center_axis',(0.,-1.,0.));
#11931=DIRECTION('ref_axis',(0.,0.,-1.));
#11932=DIRECTION('center_axis',(0.,1.,0.));
#11933=DIRECTION('ref_axis',(1.,0.,0.));
#11934=DIRECTION('center_axis',(0.,-1.,0.));
#11935=DIRECTION('ref_axis',(1.,0.,0.));
#11936=DIRECTION('center_axis',(0.,-1.,0.));
#11937=DIRECTION('ref_axis',(0.,0.,-1.));
#11938=DIRECTION('center_axis',(6.12323399573676E-17,0.,1.));
#11939=DIRECTION('ref_axis',(1.,0.,0.));
#11940=DIRECTION('center_axis',(0.,-1.,0.));
#11941=DIRECTION('ref_axis',(0.,0.,-1.));
#11942=DIRECTION('center_axis',(0.,1.,0.));
#11943=DIRECTION('ref_axis',(1.,0.,0.));
#11944=DIRECTION('center_axis',(0.,-1.,0.));
#11945=DIRECTION('ref_axis',(1.,0.,0.));
#11946=DIRECTION('center_axis',(0.,-1.,0.));
#11947=DIRECTION('ref_axis',(0.,0.,-1.));
#11948=DIRECTION('center_axis',(0.,0.,1.));
#11949=DIRECTION('ref_axis',(1.,0.,0.));
#11950=DIRECTION('center_axis',(0.,-1.,0.));
#11951=DIRECTION('ref_axis',(0.,0.,-1.));
#11952=DIRECTION('center_axis',(0.,1.,0.));
#11953=DIRECTION('ref_axis',(1.,0.,0.));
#11954=DIRECTION('center_axis',(0.,1.,0.));
#11955=DIRECTION('ref_axis',(1.,0.,0.));
#11956=DIRECTION('',(0.,1.,0.));
#11957=DIRECTION('center_axis',(0.,-1.,0.));
#11958=DIRECTION('ref_axis',(1.,0.,0.));
#11959=DIRECTION('center_axis',(0.,-1.,0.));
#11960=DIRECTION('ref_axis',(1.,0.,0.));
#11961=DIRECTION('center_axis',(0.,1.,0.));
#11962=DIRECTION('ref_axis',(1.,0.,0.));
#11963=DIRECTION('center_axis',(0.,-1.,0.));
#11964=DIRECTION('ref_axis',(0.,0.,-1.));
#11965=DIRECTION('center_axis',(0.,0.,1.));
#11966=DIRECTION('ref_axis',(1.,0.,0.));
#11967=DIRECTION('center_axis',(0.,-1.,0.));
#11968=DIRECTION('ref_axis',(0.,0.,-1.));
#11969=DIRECTION('center_axis',(0.,-1.,0.));
#11970=DIRECTION('ref_axis',(-1.,0.,0.));
#11971=DIRECTION('center_axis',(0.,1.,0.));
#11972=DIRECTION('ref_axis',(1.,0.,0.));
#11973=DIRECTION('axis',(0.,0.,1.));
#11974=DIRECTION('refdir',(1.,0.,0.));
#11975=DIRECTION('center_axis',(0.,1.,0.));
#11976=DIRECTION('ref_axis',(0.,0.,1.));
#11977=DIRECTION('center_axis',(0.,-1.,0.));
#11978=DIRECTION('ref_axis',(1.,0.,0.));
#11979=DIRECTION('center_axis',(0.,-1.,0.));
#11980=DIRECTION('ref_axis',(1.,0.,0.));
#11981=DIRECTION('center_axis',(0.,-1.,0.));
#11982=DIRECTION('ref_axis',(1.,0.,0.));
#11983=DIRECTION('center_axis',(0.,-1.,0.));
#11984=DIRECTION('ref_axis',(1.,0.,0.));
#11985=DIRECTION('',(0.,1.,0.));
#11986=DIRECTION('center_axis',(0.,-1.,0.));
#11987=DIRECTION('ref_axis',(0.,0.,-1.));
#11988=DIRECTION('center_axis',(0.,-1.,0.));
#11989=DIRECTION('ref_axis',(1.,0.,0.));
#11990=DIRECTION('center_axis',(0.,-1.,0.));
#11991=DIRECTION('ref_axis',(1.,0.,0.));
#11992=DIRECTION('',(0.,1.,0.));
#11993=DIRECTION('center_axis',(0.,1.,0.));
#11994=DIRECTION('ref_axis',(0.,0.,1.));
#11995=DIRECTION('center_axis',(0.,-1.,0.));
#11996=DIRECTION('ref_axis',(1.,0.,0.));
#11997=DIRECTION('center_axis',(0.,-1.,0.));
#11998=DIRECTION('ref_axis',(1.,0.,0.));
#11999=DIRECTION('center_axis',(0.,-1.,0.));
#12000=DIRECTION('ref_axis',(1.,0.,0.));
#12001=DIRECTION('center_axis',(0.,-1.,0.));
#12002=DIRECTION('ref_axis',(1.,0.,0.));
#12003=DIRECTION('',(0.,1.,0.));
#12004=DIRECTION('center_axis',(0.,-1.,0.));
#12005=DIRECTION('ref_axis',(0.,0.,-1.));
#12006=DIRECTION('center_axis',(0.,-1.,0.));
#12007=DIRECTION('ref_axis',(1.,0.,0.));
#12008=DIRECTION('center_axis',(0.,-1.,0.));
#12009=DIRECTION('ref_axis',(1.,0.,0.));
#12010=DIRECTION('',(0.,1.,0.));
#12011=DIRECTION('',(0.,0.,1.));
#12012=DIRECTION('',(1.,0.,0.));
#12013=DIRECTION('',(0.,0.,1.));
#12014=DIRECTION('',(1.,0.,0.));
#12015=DIRECTION('',(0.,0.,1.));
#12016=DIRECTION('',(1.,0.,0.));
#12017=DIRECTION('',(0.,0.,1.));
#12018=DIRECTION('',(1.,0.,0.));
#12019=DIRECTION('',(0.,0.,1.));
#12020=DIRECTION('',(1.,0.,0.));
#12021=DIRECTION('axis',(0.,0.,1.));
#12022=DIRECTION('refdir',(1.,0.,0.));
#12023=DIRECTION('center_axis',(0.866025403784439,0.,-0.5));
#12024=DIRECTION('ref_axis',(0.5,0.,0.866025403784439));
#12025=DIRECTION('',(-0.5,0.,-0.866025403784439));
#12026=DIRECTION('',(0.,-1.,0.));
#12027=DIRECTION('',(0.5,0.,0.866025403784439));
#12028=DIRECTION('',(0.,-1.,0.));
#12029=DIRECTION('center_axis',(1.60246890531964E-16,0.,-1.));
#12030=DIRECTION('ref_axis',(1.,0.,1.60246890531964E-16));
#12031=DIRECTION('',(-1.,0.,-1.60246890531964E-16));
#12032=DIRECTION('',(0.,-1.,0.));
#12033=DIRECTION('',(1.,0.,1.60246890531964E-16));
#12034=DIRECTION('center_axis',(-0.866025403784439,0.,-0.5));
#12035=DIRECTION('ref_axis',(0.5,0.,-0.866025403784439));
#12036=DIRECTION('',(-0.5,0.,0.866025403784439));
#12037=DIRECTION('',(0.,-1.,0.));
#12038=DIRECTION('',(0.5,0.,-0.866025403784439));
#12039=DIRECTION('center_axis',(-0.866025403784439,0.,0.5));
#12040=DIRECTION('ref_axis',(-0.5,0.,-0.866025403784439));
#12041=DIRECTION('',(0.5,0.,0.866025403784439));
#12042=DIRECTION('',(0.,-1.,0.));
#12043=DIRECTION('',(-0.5,0.,-0.866025403784439));
#12044=DIRECTION('center_axis',(-1.60246890531964E-16,0.,1.));
#12045=DIRECTION('ref_axis',(-1.,0.,-1.60246890531964E-16));
#12046=DIRECTION('',(1.,0.,1.60246890531964E-16));
#12047=DIRECTION('',(0.,-1.,0.));
#12048=DIRECTION('',(-1.,0.,-1.60246890531964E-16));
#12049=DIRECTION('center_axis',(0.866025403784439,0.,0.5));
#12050=DIRECTION('ref_axis',(-0.5,0.,0.866025403784439));
#12051=DIRECTION('',(0.5,0.,-0.866025403784439));
#12052=DIRECTION('',(-0.5,0.,0.866025403784439));
#12053=DIRECTION('center_axis',(0.,1.,0.));
#12054=DIRECTION('ref_axis',(1.,0.,0.));
#12055=DIRECTION('center_axis',(0.,-1.,0.));
#12056=DIRECTION('ref_axis',(0.,0.,-1.));
#12057=DIRECTION('center_axis',(0.,1.,0.));
#12058=DIRECTION('ref_axis',(1.,0.,0.));
#12059=DIRECTION('center_axis',(0.,1.,0.));
#12060=DIRECTION('ref_axis',(1.,0.,0.));
#12061=DIRECTION('center_axis',(0.,-1.,0.));
#12062=DIRECTION('ref_axis',(1.,0.,0.));
#12063=DIRECTION('center_axis',(0.,1.,0.));
#12064=DIRECTION('ref_axis',(1.,0.,0.));
#12065=DIRECTION('',(0.,-1.,0.));
#12066=DIRECTION('center_axis',(0.,1.,0.));
#12067=DIRECTION('ref_axis',(1.,0.,0.));
#12068=DIRECTION('center_axis',(0.,1.,0.));
#12069=DIRECTION('ref_axis',(1.,0.,0.));
#12070=DIRECTION('center_axis',(0.,1.,0.));
#12071=DIRECTION('ref_axis',(0.,0.,1.));
#12072=DIRECTION('center_axis',(0.,-1.,0.));
#12073=DIRECTION('ref_axis',(1.,0.,0.));
#12074=DIRECTION('center_axis',(0.,-1.,0.));
#12075=DIRECTION('ref_axis',(1.,0.,0.));
#12076=DIRECTION('center_axis',(0.,-1.,0.));
#12077=DIRECTION('ref_axis',(1.,0.,0.));
#12078=DIRECTION('',(0.707106781186547,0.707106781186548,8.65956056235493E-17));
#12079=DIRECTION('center_axis',(0.,-1.,0.));
#12080=DIRECTION('ref_axis',(1.,0.,0.));
#12081=DIRECTION('center_axis',(0.,-1.,0.));
#12082=DIRECTION('ref_axis',(1.,0.,0.));
#12083=DIRECTION('',(0.,1.,0.));
#12084=DIRECTION('center_axis',(0.,1.,0.));
#12085=DIRECTION('ref_axis',(1.,0.,0.));
#12086=DIRECTION('center_axis',(0.,-1.,0.));
#12087=DIRECTION('ref_axis',(1.,0.,0.));
#12088=DIRECTION('',(-0.707106781186547,0.707106781186548,-8.65956056235493E-17));
#12089=DIRECTION('center_axis',(0.,-1.,0.));
#12090=DIRECTION('ref_axis',(0.,0.,-1.));
#12091=DIRECTION('center_axis',(0.,-1.,0.));
#12092=DIRECTION('ref_axis',(1.,0.,0.));
#12093=DIRECTION('center_axis',(0.,1.,0.));
#12094=DIRECTION('ref_axis',(1.,0.,0.));
#12095=DIRECTION('center_axis',(0.,1.,0.));
#12096=DIRECTION('ref_axis',(1.,0.,0.));
#12097=DIRECTION('',(-0.447213595499958,0.894427190999916,-5.47678698264203E-17));
#12098=DIRECTION('center_axis',(0.,-1.,0.));
#12099=DIRECTION('ref_axis',(1.,0.,0.));
#12100=DIRECTION('center_axis',(0.,1.,0.));
#12101=DIRECTION('ref_axis',(1.,0.,0.));
#12102=DIRECTION('',(0.,1.,0.));
#12103=DIRECTION('center_axis',(0.,1.,0.));
#12104=DIRECTION('ref_axis',(1.,0.,0.));
#12105=DIRECTION('',(-0.707106781186547,0.707106781186548,-8.65956056235493E-17));
#12106=DIRECTION('axis',(0.,0.,1.));
#12107=DIRECTION('refdir',(1.,0.,0.));
#12108=DIRECTION('axis',(0.,0.,1.));
#12109=DIRECTION('refdir',(1.,0.,0.));
#12110=DIRECTION('center_axis',(0.,-1.,0.));
#12111=DIRECTION('ref_axis',(0.,0.,-1.));
#12112=DIRECTION('center_axis',(0.,-1.,0.));
#12113=DIRECTION('ref_axis',(1.,0.,0.));
#12114=DIRECTION('center_axis',(0.,-1.,0.));
#12115=DIRECTION('ref_axis',(1.,0.,0.));
#12116=DIRECTION('center_axis',(1.,0.,1.22464679914735E-16));
#12117=DIRECTION('ref_axis',(-1.22464679914735E-16,0.,1.));
#12118=DIRECTION('center_axis',(0.,1.,0.));
#12119=DIRECTION('ref_axis',(1.,0.,0.));
#12120=DIRECTION('center_axis',(0.,1.,0.));
#12121=DIRECTION('ref_axis',(1.,0.,0.));
#12122=DIRECTION('center_axis',(0.,-1.,0.));
#12123=DIRECTION('ref_axis',(1.,0.,0.));
#12124=DIRECTION('',(0.,1.,0.));
#12125=DIRECTION('center_axis',(0.,-1.,0.));
#12126=DIRECTION('ref_axis',(1.,0.,0.));
#12127=DIRECTION('center_axis',(0.,-1.,0.));
#12128=DIRECTION('ref_axis',(1.,0.,0.));
#12129=DIRECTION('center_axis',(0.,-1.,0.));
#12130=DIRECTION('ref_axis',(1.,0.,0.));
#12131=DIRECTION('',(0.,1.,0.));
#12132=DIRECTION('center_axis',(0.,-1.,0.));
#12133=DIRECTION('ref_axis',(1.,0.,0.));
#12134=DIRECTION('center_axis',(0.,1.,0.));
#12135=DIRECTION('ref_axis',(1.,0.,0.));
#12136=DIRECTION('',(-0.707106781186548,0.707106781186547,-8.65956056235493E-17));
#12137=DIRECTION('center_axis',(0.,-1.,0.));
#12138=DIRECTION('ref_axis',(1.,0.,0.));
#12139=DIRECTION('center_axis',(0.,1.,0.));
#12140=DIRECTION('ref_axis',(0.,0.,1.));
#12141=DIRECTION('center_axis',(0.,-1.,0.));
#12142=DIRECTION('ref_axis',(1.,0.,0.));
#12143=DIRECTION('center_axis',(0.,-1.,0.));
#12144=DIRECTION('ref_axis',(1.,0.,0.));
#12145=DIRECTION('',(0.,1.,0.));
#12146=DIRECTION('center_axis',(0.,-1.,0.));
#12147=DIRECTION('ref_axis',(0.,0.,-1.));
#12148=DIRECTION('center_axis',(0.,-1.,0.));
#12149=DIRECTION('ref_axis',(1.,0.,0.));
#12150=DIRECTION('center_axis',(0.,-1.,0.));
#12151=DIRECTION('ref_axis',(1.,0.,0.));
#12152=DIRECTION('',(0.707106781186548,0.707106781186547,8.65956056235493E-17));
#12153=DIRECTION('axis',(0.,0.,1.));
#12154=DIRECTION('refdir',(1.,0.,0.));
#12155=DIRECTION('center_axis',(0.,-1.,0.));
#12156=DIRECTION('ref_axis',(0.,0.,-1.));
#12157=DIRECTION('center_axis',(0.,-1.,0.));
#12158=DIRECTION('ref_axis',(1.,0.,0.));
#12159=DIRECTION('center_axis',(0.,-1.,0.));
#12160=DIRECTION('ref_axis',(1.,0.,0.));
#12161=DIRECTION('center_axis',(1.,0.,1.22464679914735E-16));
#12162=DIRECTION('ref_axis',(-1.22464679914735E-16,0.,1.));
#12163=DIRECTION('center_axis',(0.,1.,0.));
#12164=DIRECTION('ref_axis',(1.,0.,0.));
#12165=DIRECTION('center_axis',(0.,1.,0.));
#12166=DIRECTION('ref_axis',(1.,0.,0.));
#12167=DIRECTION('center_axis',(0.,-1.,0.));
#12168=DIRECTION('ref_axis',(1.,0.,0.));
#12169=DIRECTION('center_axis',(0.,-1.,0.));
#12170=DIRECTION('ref_axis',(1.,0.,0.));
#12171=DIRECTION('',(0.,1.,0.));
#12172=DIRECTION('center_axis',(0.,1.,0.));
#12173=DIRECTION('ref_axis',(0.,0.,1.));
#12174=DIRECTION('center_axis',(0.,-1.,0.));
#12175=DIRECTION('ref_axis',(1.,0.,0.));
#12176=DIRECTION('center_axis',(0.,-1.,0.));
#12177=DIRECTION('ref_axis',(1.,0.,0.));
#12178=DIRECTION('center_axis',(0.,-1.,0.));
#12179=DIRECTION('ref_axis',(1.,0.,0.));
#12180=DIRECTION('center_axis',(0.,-1.,0.));
#12181=DIRECTION('ref_axis',(1.,0.,0.));
#12182=DIRECTION('',(0.707106781186548,0.707106781186547,8.65956056235494E-17));
#12183=DIRECTION('center_axis',(0.,-1.,0.));
#12184=DIRECTION('ref_axis',(1.,0.,0.));
#12185=DIRECTION('center_axis',(0.,-1.,0.));
#12186=DIRECTION('ref_axis',(1.,0.,0.));
#12187=DIRECTION('',(0.,1.,0.));
#12188=DIRECTION('center_axis',(0.,1.,0.));
#12189=DIRECTION('ref_axis',(1.,0.,0.));
#12190=DIRECTION('center_axis',(0.,-1.,0.));
#12191=DIRECTION('ref_axis',(1.,0.,0.));
#12192=DIRECTION('',(-0.707106781186548,0.707106781186547,-8.65956056235494E-17));
#12193=DIRECTION('center_axis',(0.,-1.,0.));
#12194=DIRECTION('ref_axis',(0.,0.,-1.));
#12195=DIRECTION('center_axis',(0.,-1.,0.));
#12196=DIRECTION('ref_axis',(1.,0.,0.));
#12197=DIRECTION('',(0.,1.,0.));
#12198=DIRECTION('axis',(0.,0.,1.));
#12199=DIRECTION('refdir',(1.,0.,0.));
#12200=DIRECTION('center_axis',(0.,0.,1.));
#12201=DIRECTION('ref_axis',(1.,0.,0.));
#12202=DIRECTION('center_axis',(1.22464679914735E-16,-1.,0.));
#12203=DIRECTION('ref_axis',(-1.,-1.22464679914735E-16,0.));
#12204=DIRECTION('center_axis',(0.78183148246803,0.,0.623489801858733));
#12205=DIRECTION('ref_axis',(0.623489801858734,0.,-0.78183148246803));
#12206=DIRECTION('center_axis',(7.63554790147315E-17,-1.,-9.57467422477103E-17));
#12207=DIRECTION('ref_axis',(-0.623489801858734,-1.22464679914735E-16,0.78183148246803));
#12208=DIRECTION('center_axis',(0.974927912181824,0.,-0.222520933956314));
#12209=DIRECTION('ref_axis',(-0.222520933956314,0.,-0.974927912181824));
#12210=DIRECTION('center_axis',(-2.7250954951288E-17,-1.,-1.19394234705288E-16));
#12211=DIRECTION('ref_axis',(0.222520933956314,-1.22464679914735E-16,0.974927912181824));
#12212=DIRECTION('center_axis',(0.433883739117558,0.,-0.900968867902419));
#12213=DIRECTION('ref_axis',(-0.900968867902419,0.,-0.433883739117558));
#12214=DIRECTION('center_axis',(-1.10336864020811E-16,-1.,-5.31354332312403E-17));
#12215=DIRECTION('ref_axis',(0.900968867902419,-1.22464679914735E-16,0.433883739117558));
#12216=DIRECTION('center_axis',(-0.433883739117558,0.,-0.900968867902419));
#12217=DIRECTION('ref_axis',(-0.900968867902419,0.,0.433883739117558));
#12218=DIRECTION('center_axis',(-1.10336864020811E-16,-1.,5.31354332312403E-17));
#12219=DIRECTION('ref_axis',(0.900968867902419,-1.22464679914735E-16,-0.433883739117558));
#12220=DIRECTION('center_axis',(-0.974927912181824,0.,-0.222520933956314));
#12221=DIRECTION('ref_axis',(-0.222520933956315,0.,0.974927912181824));
#12222=DIRECTION('center_axis',(-2.7250954951288E-17,-1.,1.19394234705288E-16));
#12223=DIRECTION('ref_axis',(0.222520933956315,-1.22464679914735E-16,-0.974927912181824));
#12224=DIRECTION('center_axis',(-0.78183148246803,0.,0.623489801858734));
#12225=DIRECTION('ref_axis',(0.623489801858733,0.,0.78183148246803));
#12226=DIRECTION('center_axis',(7.63554790147315E-17,-1.,9.57467422477103E-17));
#12227=DIRECTION('ref_axis',(-0.623489801858733,-1.22464679914735E-16,-0.78183148246803));
#12228=DIRECTION('axis',(0.,0.,1.));
#12229=DIRECTION('refdir',(1.,0.,0.));
#12230=DIRECTION('center_axis',(0.,0.,1.));
#12231=DIRECTION('ref_axis',(1.,0.,0.));
#12232=DIRECTION('center_axis',(0.,-1.,0.));
#12233=DIRECTION('ref_axis',(0.,0.,-1.));
#12234=DIRECTION('center_axis',(0.,-1.,0.));
#12235=DIRECTION('ref_axis',(0.,0.,-1.));
#12236=DIRECTION('center_axis',(0.,1.,0.));
#12237=DIRECTION('ref_axis',(1.,0.,0.));
#12238=DIRECTION('center_axis',(0.,1.,0.));
#12239=DIRECTION('ref_axis',(1.,0.,0.));
#12240=DIRECTION('center_axis',(0.,1.,0.));
#12241=DIRECTION('ref_axis',(1.,0.,0.));
#12242=DIRECTION('center_axis',(0.,1.,0.));
#12243=DIRECTION('ref_axis',(1.,0.,0.));
#12244=DIRECTION('',(0.,-1.,0.));
#12245=DIRECTION('center_axis',(0.,-1.,0.));
#12246=DIRECTION('ref_axis',(1.,0.,0.));
#12247=DIRECTION('center_axis',(0.,1.,0.));
#12248=DIRECTION('ref_axis',(1.,0.,0.));
#12249=DIRECTION('center_axis',(0.,1.,0.));
#12250=DIRECTION('ref_axis',(1.,0.,0.));
#12251=DIRECTION('center_axis',(0.,1.,0.));
#12252=DIRECTION('ref_axis',(1.,0.,0.));
#12253=DIRECTION('center_axis',(0.,1.,0.));
#12254=DIRECTION('ref_axis',(1.,0.,0.));
#12255=DIRECTION('center_axis',(0.,1.,0.));
#12256=DIRECTION('ref_axis',(1.,0.,0.));
#12257=DIRECTION('center_axis',(0.,1.,0.));
#12258=DIRECTION('ref_axis',(1.,0.,0.));
#12259=DIRECTION('center_axis',(0.,-1.,0.));
#12260=DIRECTION('ref_axis',(1.,0.,0.));
#12261=DIRECTION('center_axis',(0.,-1.,0.));
#12262=DIRECTION('ref_axis',(0.,0.,-1.));
#12263=DIRECTION('center_axis',(8.96625347776458E-17,0.,1.));
#12264=DIRECTION('ref_axis',(1.,0.,0.));
#12265=DIRECTION('center_axis',(0.,-1.,0.));
#12266=DIRECTION('ref_axis',(0.,0.,-1.));
#12267=DIRECTION('center_axis',(0.,1.,0.));
#12268=DIRECTION('ref_axis',(1.,0.,0.));
#12269=DIRECTION('center_axis',(0.,-1.,0.));
#12270=DIRECTION('ref_axis',(1.,0.,0.));
#12271=DIRECTION('center_axis',(0.,-1.,0.));
#12272=DIRECTION('ref_axis',(0.,0.,-1.));
#12273=DIRECTION('center_axis',(0.,0.,1.));
#12274=DIRECTION('ref_axis',(1.,0.,0.));
#12275=DIRECTION('center_axis',(0.,-1.,0.));
#12276=DIRECTION('ref_axis',(0.,0.,-1.));
#12277=DIRECTION('center_axis',(0.,1.,0.));
#12278=DIRECTION('ref_axis',(1.,0.,0.));
#12279=DIRECTION('center_axis',(0.,-1.,0.));
#12280=DIRECTION('ref_axis',(1.,0.,0.));
#12281=DIRECTION('center_axis',(0.,-1.,0.));
#12282=DIRECTION('ref_axis',(1.,0.,0.));
#12283=DIRECTION('center_axis',(0.,-1.,0.));
#12284=DIRECTION('ref_axis',(0.,0.,-1.));
#12285=DIRECTION('center_axis',(0.,0.,1.));
#12286=DIRECTION('ref_axis',(1.,0.,0.));
#12287=DIRECTION('center_axis',(0.,-1.,0.));
#12288=DIRECTION('ref_axis',(0.,0.,-1.));
#12289=DIRECTION('center_axis',(0.,1.,0.));
#12290=DIRECTION('ref_axis',(1.,0.,0.));
#12291=DIRECTION('center_axis',(0.,-1.,0.));
#12292=DIRECTION('ref_axis',(1.,0.,0.));
#12293=DIRECTION('center_axis',(0.,-1.,0.));
#12294=DIRECTION('ref_axis',(0.,0.,-1.));
#12295=DIRECTION('center_axis',(8.96625347776458E-17,0.,1.));
#12296=DIRECTION('ref_axis',(1.,0.,0.));
#12297=DIRECTION('center_axis',(0.,-1.,0.));
#12298=DIRECTION('ref_axis',(0.,0.,-1.));
#12299=DIRECTION('center_axis',(0.,1.,0.));
#12300=DIRECTION('ref_axis',(1.,0.,0.));
#12301=DIRECTION('center_axis',(0.,-1.,0.));
#12302=DIRECTION('ref_axis',(1.,0.,0.));
#12303=DIRECTION('center_axis',(0.,-1.,0.));
#12304=DIRECTION('ref_axis',(0.,0.,-1.));
#12305=DIRECTION('center_axis',(0.,0.,1.));
#12306=DIRECTION('ref_axis',(1.,0.,0.));
#12307=DIRECTION('center_axis',(0.,-1.,0.));
#12308=DIRECTION('ref_axis',(0.,0.,-1.));
#12309=DIRECTION('center_axis',(0.,1.,0.));
#12310=DIRECTION('ref_axis',(1.,0.,0.));
#12311=DIRECTION('center_axis',(0.,1.,0.));
#12312=DIRECTION('ref_axis',(1.,0.,0.));
#12313=DIRECTION('',(0.,1.,0.));
#12314=DIRECTION('center_axis',(0.,-1.,0.));
#12315=DIRECTION('ref_axis',(1.,0.,0.));
#12316=DIRECTION('center_axis',(0.,-1.,0.));
#12317=DIRECTION('ref_axis',(1.,0.,0.));
#12318=DIRECTION('center_axis',(0.,1.,0.));
#12319=DIRECTION('ref_axis',(1.,0.,0.));
#12320=DIRECTION('center_axis',(0.,-1.,0.));
#12321=DIRECTION('ref_axis',(0.,0.,-1.));
#12322=DIRECTION('center_axis',(0.,0.,1.));
#12323=DIRECTION('ref_axis',(1.,0.,0.));
#12324=DIRECTION('center_axis',(0.,-1.,0.));
#12325=DIRECTION('ref_axis',(0.,0.,-1.));
#12326=DIRECTION('center_axis',(0.,-1.,0.));
#12327=DIRECTION('ref_axis',(-1.,0.,0.));
#12328=DIRECTION('center_axis',(0.,1.,0.));
#12329=DIRECTION('ref_axis',(1.,0.,0.));
#12330=DIRECTION('axis',(0.,0.,1.));
#12331=DIRECTION('refdir',(1.,0.,0.));
#12332=DIRECTION('center_axis',(0.,1.,0.));
#12333=DIRECTION('ref_axis',(0.,0.,1.));
#12334=DIRECTION('center_axis',(0.,-1.,0.));
#12335=DIRECTION('ref_axis',(1.,0.,0.));
#12336=DIRECTION('center_axis',(0.,-1.,0.));
#12337=DIRECTION('ref_axis',(1.,0.,0.));
#12338=DIRECTION('center_axis',(0.,-1.,0.));
#12339=DIRECTION('ref_axis',(1.,0.,0.));
#12340=DIRECTION('center_axis',(0.,-1.,0.));
#12341=DIRECTION('ref_axis',(1.,0.,0.));
#12342=DIRECTION('',(0.,1.,0.));
#12343=DIRECTION('center_axis',(0.,-1.,0.));
#12344=DIRECTION('ref_axis',(0.,0.,-1.));
#12345=DIRECTION('center_axis',(0.,-1.,0.));
#12346=DIRECTION('ref_axis',(1.,0.,0.));
#12347=DIRECTION('center_axis',(0.,-1.,0.));
#12348=DIRECTION('ref_axis',(1.,0.,0.));
#12349=DIRECTION('',(0.,1.,0.));
#12350=DIRECTION('center_axis',(0.,1.,0.));
#12351=DIRECTION('ref_axis',(0.,0.,1.));
#12352=DIRECTION('center_axis',(0.,-1.,0.));
#12353=DIRECTION('ref_axis',(1.,0.,0.));
#12354=DIRECTION('center_axis',(0.,-1.,0.));
#12355=DIRECTION('ref_axis',(1.,0.,0.));
#12356=DIRECTION('center_axis',(0.,-1.,0.));
#12357=DIRECTION('ref_axis',(1.,0.,0.));
#12358=DIRECTION('center_axis',(0.,-1.,0.));
#12359=DIRECTION('ref_axis',(1.,0.,0.));
#12360=DIRECTION('',(0.,1.,0.));
#12361=DIRECTION('center_axis',(0.,-1.,0.));
#12362=DIRECTION('ref_axis',(0.,0.,-1.));
#12363=DIRECTION('center_axis',(0.,-1.,0.));
#12364=DIRECTION('ref_axis',(1.,0.,0.));
#12365=DIRECTION('center_axis',(0.,-1.,0.));
#12366=DIRECTION('ref_axis',(1.,0.,0.));
#12367=DIRECTION('',(0.,1.,0.));
#12368=DIRECTION('',(0.,0.,1.));
#12369=DIRECTION('',(1.,0.,0.));
#12370=DIRECTION('',(0.,0.,1.));
#12371=DIRECTION('',(1.,0.,0.));
#12372=DIRECTION('',(0.,0.,1.));
#12373=DIRECTION('',(1.,0.,0.));
#12374=DIRECTION('',(0.,0.,1.));
#12375=DIRECTION('',(1.,0.,0.));
#12376=DIRECTION('',(0.,0.,1.));
#12377=DIRECTION('',(1.,0.,0.));
#12378=DIRECTION('axis',(0.,0.,1.));
#12379=DIRECTION('refdir',(1.,0.,0.));
#12380=DIRECTION('center_axis',(0.866025403784439,0.,-0.5));
#12381=DIRECTION('ref_axis',(0.5,0.,0.866025403784439));
#12382=DIRECTION('',(-0.5,0.,-0.866025403784439));
#12383=DIRECTION('',(0.,-1.,0.));
#12384=DIRECTION('',(0.5,0.,0.866025403784439));
#12385=DIRECTION('',(0.,-1.,0.));
#12386=DIRECTION('center_axis',(1.60246890531964E-16,0.,-1.));
#12387=DIRECTION('ref_axis',(1.,0.,1.60246890531964E-16));
#12388=DIRECTION('',(-1.,0.,-1.60246890531964E-16));
#12389=DIRECTION('',(0.,-1.,0.));
#12390=DIRECTION('',(1.,0.,1.60246890531964E-16));
#12391=DIRECTION('center_axis',(-0.866025403784439,0.,-0.5));
#12392=DIRECTION('ref_axis',(0.5,0.,-0.866025403784439));
#12393=DIRECTION('',(-0.5,0.,0.866025403784439));
#12394=DIRECTION('',(0.,-1.,0.));
#12395=DIRECTION('',(0.5,0.,-0.866025403784439));
#12396=DIRECTION('center_axis',(-0.866025403784439,0.,0.5));
#12397=DIRECTION('ref_axis',(-0.5,0.,-0.866025403784439));
#12398=DIRECTION('',(0.5,0.,0.866025403784439));
#12399=DIRECTION('',(0.,-1.,0.));
#12400=DIRECTION('',(-0.5,0.,-0.866025403784439));
#12401=DIRECTION('center_axis',(-1.60246890531964E-16,0.,1.));
#12402=DIRECTION('ref_axis',(-1.,0.,-1.60246890531964E-16));
#12403=DIRECTION('',(1.,0.,1.60246890531964E-16));
#12404=DIRECTION('',(0.,-1.,0.));
#12405=DIRECTION('',(-1.,0.,-1.60246890531964E-16));
#12406=DIRECTION('center_axis',(0.866025403784439,0.,0.5));
#12407=DIRECTION('ref_axis',(-0.5,0.,0.866025403784439));
#12408=DIRECTION('',(0.5,0.,-0.866025403784439));
#12409=DIRECTION('',(-0.5,0.,0.866025403784439));
#12410=DIRECTION('center_axis',(0.,1.,0.));
#12411=DIRECTION('ref_axis',(1.,0.,0.));
#12412=DIRECTION('center_axis',(0.,-1.,0.));
#12413=DIRECTION('ref_axis',(0.,0.,-1.));
#12414=DIRECTION('center_axis',(0.,1.,0.));
#12415=DIRECTION('ref_axis',(1.,0.,0.));
#12416=DIRECTION('center_axis',(0.,1.,0.));
#12417=DIRECTION('ref_axis',(1.,0.,0.));
#12418=DIRECTION('center_axis',(0.,1.,0.));
#12419=DIRECTION('ref_axis',(0.,0.,1.));
#12420=DIRECTION('center_axis',(0.,-1.,0.));
#12421=DIRECTION('ref_axis',(1.,0.,0.));
#12422=DIRECTION('center_axis',(0.,-1.,0.));
#12423=DIRECTION('ref_axis',(1.,0.,0.));
#12424=DIRECTION('center_axis',(0.,-1.,0.));
#12425=DIRECTION('ref_axis',(1.,0.,0.));
#12426=DIRECTION('',(0.707106781186547,0.707106781186548,8.65956056235493E-17));
#12427=DIRECTION('center_axis',(0.,-1.,0.));
#12428=DIRECTION('ref_axis',(1.,0.,0.));
#12429=DIRECTION('center_axis',(0.,-1.,0.));
#12430=DIRECTION('ref_axis',(1.,0.,0.));
#12431=DIRECTION('',(0.,1.,0.));
#12432=DIRECTION('center_axis',(0.,1.,0.));
#12433=DIRECTION('ref_axis',(1.,0.,0.));
#12434=DIRECTION('center_axis',(0.,-1.,0.));
#12435=DIRECTION('ref_axis',(1.,0.,0.));
#12436=DIRECTION('',(-0.707106781186547,0.707106781186548,-8.65956056235493E-17));
#12437=DIRECTION('center_axis',(0.,-1.,0.));
#12438=DIRECTION('ref_axis',(0.,0.,-1.));
#12439=DIRECTION('center_axis',(0.,-1.,0.));
#12440=DIRECTION('ref_axis',(1.,0.,0.));
#12441=DIRECTION('center_axis',(0.,1.,0.));
#12442=DIRECTION('ref_axis',(1.,0.,0.));
#12443=DIRECTION('center_axis',(0.,1.,0.));
#12444=DIRECTION('ref_axis',(1.,0.,0.));
#12445=DIRECTION('',(-0.447213595499958,0.894427190999916,-5.47678698264203E-17));
#12446=DIRECTION('center_axis',(0.,-1.,0.));
#12447=DIRECTION('ref_axis',(1.,0.,0.));
#12448=DIRECTION('',(0.,1.,0.));
#12449=DIRECTION('axis',(0.,0.,1.));
#12450=DIRECTION('refdir',(1.,0.,0.));
#12451=DIRECTION('axis',(0.,0.,1.));
#12452=DIRECTION('refdir',(1.,0.,0.));
#12453=DIRECTION('center_axis',(0.,1.,0.));
#12454=DIRECTION('ref_axis',(1.,0.,0.));
#12455=DIRECTION('center_axis',(0.,1.,0.));
#12456=DIRECTION('ref_axis',(1.,0.,0.));
#12457=DIRECTION('',(0.,1.,0.));
#12458=DIRECTION('center_axis',(0.,1.,0.));
#12459=DIRECTION('ref_axis',(1.,0.,0.));
#12460=DIRECTION('center_axis',(0.,1.,0.));
#12461=DIRECTION('ref_axis',(1.,0.,0.));
#12462=DIRECTION('center_axis',(0.,1.,0.));
#12463=DIRECTION('ref_axis',(1.,0.,0.));
#12464=DIRECTION('center_axis',(0.,1.,0.));
#12465=DIRECTION('ref_axis',(1.,0.,0.));
#12466=DIRECTION('center_axis',(0.,1.,0.));
#12467=DIRECTION('ref_axis',(1.,0.,0.));
#12468=DIRECTION('center_axis',(0.,1.,0.));
#12469=DIRECTION('ref_axis',(1.,0.,0.));
#12470=DIRECTION('center_axis',(0.,1.,0.));
#12471=DIRECTION('ref_axis',(1.,0.,0.));
#12472=DIRECTION('center_axis',(0.,-1.,0.));
#12473=DIRECTION('ref_axis',(1.,0.,0.));
#12474=DIRECTION('center_axis',(0.,1.,0.));
#12475=DIRECTION('ref_axis',(1.,0.,0.));
#12476=DIRECTION('',(0.,-1.,0.));
#12477=DIRECTION('center_axis',(0.,1.,0.));
#12478=DIRECTION('ref_axis',(1.,0.,0.));
#12479=DIRECTION('',(0.,-1.,0.));
#12480=DIRECTION('center_axis',(0.,1.,0.));
#12481=DIRECTION('ref_axis',(1.,0.,0.));
#12482=DIRECTION('center_axis',(0.,1.,0.));
#12483=DIRECTION('ref_axis',(1.,0.,0.));
#12484=DIRECTION('center_axis',(0.,1.,0.));
#12485=DIRECTION('ref_axis',(1.,0.,0.));
#12486=DIRECTION('',(0.,-1.,0.));
#12487=DIRECTION('center_axis',(0.,1.,0.));
#12488=DIRECTION('ref_axis',(1.,0.,0.));
#12489=DIRECTION('center_axis',(0.,1.,0.));
#12490=DIRECTION('ref_axis',(1.,0.,0.));
#12491=DIRECTION('center_axis',(0.,1.,0.));
#12492=DIRECTION('ref_axis',(1.,0.,0.));
#12493=DIRECTION('center_axis',(0.,1.,0.));
#12494=DIRECTION('ref_axis',(1.,0.,0.));
#12495=DIRECTION('',(0.,-1.,0.));
#12496=DIRECTION('center_axis',(0.,1.,0.));
#12497=DIRECTION('ref_axis',(1.,0.,0.));
#12498=DIRECTION('center_axis',(0.,1.,0.));
#12499=DIRECTION('ref_axis',(1.,0.,0.));
#12500=DIRECTION('axis',(0.,0.,1.));
#12501=DIRECTION('refdir',(1.,0.,0.));
#12502=DIRECTION('center_axis',(0.,1.,0.));
#12503=DIRECTION('ref_axis',(1.,0.,0.));
#12504=DIRECTION('center_axis',(0.,1.,0.));
#12505=DIRECTION('ref_axis',(1.,0.,0.));
#12506=DIRECTION('',(0.,1.,0.));
#12507=DIRECTION('center_axis',(0.,-1.,0.));
#12508=DIRECTION('ref_axis',(1.,0.,0.));
#12509=DIRECTION('center_axis',(0.,1.,0.));
#12510=DIRECTION('ref_axis',(1.,0.,0.));
#12511=DIRECTION('center_axis',(0.,1.,0.));
#12512=DIRECTION('ref_axis',(1.,0.,0.));
#12513=DIRECTION('center_axis',(0.,1.,0.));
#12514=DIRECTION('ref_axis',(1.,0.,0.));
#12515=DIRECTION('',(0.,-1.,0.));
#12516=DIRECTION('center_axis',(0.,-1.,0.));
#12517=DIRECTION('ref_axis',(1.,0.,0.));
#12518=DIRECTION('center_axis',(0.,1.,0.));
#12519=DIRECTION('ref_axis',(1.,0.,0.));
#12520=DIRECTION('center_axis',(0.,1.,0.));
#12521=DIRECTION('ref_axis',(1.,0.,0.));
#12522=DIRECTION('',(0.,-1.,0.));
#12523=DIRECTION('center_axis',(0.,1.,0.));
#12524=DIRECTION('ref_axis',(1.,0.,0.));
#12525=DIRECTION('center_axis',(0.,1.,0.));
#12526=DIRECTION('ref_axis',(1.,0.,0.));
#12527=DIRECTION('center_axis',(0.,1.,0.));
#12528=DIRECTION('ref_axis',(1.,0.,0.));
#12529=DIRECTION('axis',(0.,0.,1.));
#12530=DIRECTION('refdir',(1.,0.,0.));
#12531=DIRECTION('center_axis',(0.,1.,0.));
#12532=DIRECTION('ref_axis',(1.,0.,0.));
#12533=DIRECTION('center_axis',(0.,-1.,0.));
#12534=DIRECTION('ref_axis',(1.,0.,0.));
#12535=DIRECTION('',(0.,-1.,0.));
#12536=DIRECTION('center_axis',(0.,-1.,0.));
#12537=DIRECTION('ref_axis',(1.,0.,0.));
#12538=DIRECTION('center_axis',(0.,1.,0.));
#12539=DIRECTION('ref_axis',(1.,0.,0.));
#12540=DIRECTION('center_axis',(0.,1.,0.));
#12541=DIRECTION('ref_axis',(1.,0.,0.));
#12542=DIRECTION('',(0.,-1.,0.));
#12543=DIRECTION('center_axis',(0.,1.,0.));
#12544=DIRECTION('ref_axis',(1.,0.,0.));
#12545=DIRECTION('center_axis',(0.,1.,0.));
#12546=DIRECTION('ref_axis',(1.,0.,0.));
#12547=DIRECTION('center_axis',(0.,1.,0.));
#12548=DIRECTION('ref_axis',(1.,0.,0.));
#12549=DIRECTION('axis',(0.,0.,1.));
#12550=DIRECTION('refdir',(1.,0.,0.));
#12551=DIRECTION('center_axis',(0.,0.,1.));
#12552=DIRECTION('ref_axis',(1.,0.,0.));
#12553=DIRECTION('center_axis',(0.,0.,1.));
#12554=DIRECTION('ref_axis',(1.,0.,0.));
#12555=DIRECTION('',(0.,0.,-1.));
#12556=DIRECTION('center_axis',(0.,0.,1.));
#12557=DIRECTION('ref_axis',(1.,0.,0.));
#12558=DIRECTION('center_axis',(0.,0.,1.));
#12559=DIRECTION('ref_axis',(1.,0.,0.));
#12560=DIRECTION('center_axis',(0.,0.,1.));
#12561=DIRECTION('ref_axis',(1.,0.,0.));
#12562=DIRECTION('axis',(0.,0.,1.));
#12563=DIRECTION('refdir',(1.,0.,0.));
#12564=DIRECTION('center_axis',(0.,0.,1.));
#12565=DIRECTION('ref_axis',(1.,0.,0.));
#12566=DIRECTION('center_axis',(0.,0.,1.));
#12567=DIRECTION('ref_axis',(1.,0.,0.));
#12568=DIRECTION('',(0.,0.,-1.));
#12569=DIRECTION('center_axis',(0.,0.,1.));
#12570=DIRECTION('ref_axis',(1.,0.,0.));
#12571=DIRECTION('center_axis',(0.,0.,1.));
#12572=DIRECTION('ref_axis',(1.,0.,0.));
#12573=DIRECTION('center_axis',(0.,0.,1.));
#12574=DIRECTION('ref_axis',(1.,0.,0.));
#12575=DIRECTION('axis',(0.,0.,1.));
#12576=DIRECTION('refdir',(1.,0.,0.));
#12577=DIRECTION('center_axis',(0.,1.,0.));
#12578=DIRECTION('ref_axis',(1.,0.,0.));
#12579=DIRECTION('center_axis',(0.,-1.,0.));
#12580=DIRECTION('ref_axis',(1.,0.,0.));
#12581=DIRECTION('',(0.,-1.,0.));
#12582=DIRECTION('center_axis',(0.,-1.,0.));
#12583=DIRECTION('ref_axis',(1.,0.,0.));
#12584=DIRECTION('center_axis',(0.,1.,0.));
#12585=DIRECTION('ref_axis',(1.,0.,0.));
#12586=DIRECTION('center_axis',(0.,1.,0.));
#12587=DIRECTION('ref_axis',(1.,0.,0.));
#12588=DIRECTION('',(0.,-1.,0.));
#12589=DIRECTION('center_axis',(0.,1.,0.));
#12590=DIRECTION('ref_axis',(1.,0.,0.));
#12591=DIRECTION('center_axis',(0.,1.,0.));
#12592=DIRECTION('ref_axis',(1.,0.,0.));
#12593=DIRECTION('center_axis',(0.,1.,0.));
#12594=DIRECTION('ref_axis',(1.,0.,0.));
#12595=DIRECTION('axis',(0.,0.,1.));
#12596=DIRECTION('refdir',(1.,0.,0.));
#12597=DIRECTION('center_axis',(1.,0.,6.12323399573677E-17));
#12598=DIRECTION('ref_axis',(6.12323399573677E-17,0.,-1.));
#12599=DIRECTION('',(1.,0.,6.12323399573677E-17));
#12600=DIRECTION('center_axis',(1.,0.,6.12323399573677E-17));
#12601=DIRECTION('ref_axis',(6.12323399573677E-17,0.,-1.));
#12602=DIRECTION('',(1.,0.,6.12323399573677E-17));
#12603=DIRECTION('center_axis',(0.,-1.,0.));
#12604=DIRECTION('ref_axis',(1.,0.,0.));
#12605=DIRECTION('center_axis',(0.,-1.,0.));
#12606=DIRECTION('ref_axis',(1.,0.,0.));
#12607=DIRECTION('',(0.,1.,0.));
#12608=DIRECTION('',(0.,1.,0.));
#12609=DIRECTION('center_axis',(0.,1.,0.));
#12610=DIRECTION('ref_axis',(1.,0.,0.));
#12611=DIRECTION('center_axis',(0.,0.,1.));
#12612=DIRECTION('ref_axis',(1.,0.,0.));
#12613=DIRECTION('',(0.,0.,1.));
#12614=DIRECTION('center_axis',(0.,0.,1.));
#12615=DIRECTION('ref_axis',(1.,0.,0.));
#12616=DIRECTION('',(0.,0.,1.));
#12617=DIRECTION('center_axis',(0.,1.,0.));
#12618=DIRECTION('ref_axis',(1.,0.,0.));
#12619=DIRECTION('center_axis',(0.,1.,0.));
#12620=DIRECTION('ref_axis',(1.,0.,0.));
#12621=DIRECTION('',(0.,1.,0.));
#12622=DIRECTION('',(0.,1.,0.));
#12623=DIRECTION('center_axis',(0.,-1.,0.));
#12624=DIRECTION('ref_axis',(1.,0.,0.));
#12625=DIRECTION('center_axis',(0.,1.,0.));
#12626=DIRECTION('ref_axis',(1.,0.,0.));
#12627=DIRECTION('center_axis',(0.,1.,0.));
#12628=DIRECTION('ref_axis',(1.,0.,0.));
#12629=DIRECTION('center_axis',(0.,1.,0.));
#12630=DIRECTION('ref_axis',(1.,0.,0.));
#12631=DIRECTION('center_axis',(0.,1.,0.));
#12632=DIRECTION('ref_axis',(0.951056516295154,0.,0.309016994374948));
#12633=DIRECTION('center_axis',(0.,1.,0.));
#12634=DIRECTION('ref_axis',(1.,0.,0.));
#12635=DIRECTION('center_axis',(0.,1.,0.));
#12636=DIRECTION('ref_axis',(0.809016994374947,0.,0.587785252292473));
#12637=DIRECTION('center_axis',(0.,1.,0.));
#12638=DIRECTION('ref_axis',(1.,0.,0.));
#12639=DIRECTION('center_axis',(0.,1.,0.));
#12640=DIRECTION('ref_axis',(0.587785252292473,0.,0.809016994374948));
#12641=DIRECTION('center_axis',(0.,1.,0.));
#12642=DIRECTION('ref_axis',(1.,0.,0.));
#12643=DIRECTION('center_axis',(0.,1.,0.));
#12644=DIRECTION('ref_axis',(0.309016994374947,0.,0.951056516295154));
#12645=DIRECTION('center_axis',(0.,1.,0.));
#12646=DIRECTION('ref_axis',(1.,0.,0.));
#12647=DIRECTION('center_axis',(0.,1.,0.));
#12648=DIRECTION('ref_axis',(-1.83697019872103E-16,0.,1.));
#12649=DIRECTION('center_axis',(0.,1.,0.));
#12650=DIRECTION('ref_axis',(1.,0.,0.));
#12651=DIRECTION('center_axis',(0.,1.,0.));
#12652=DIRECTION('ref_axis',(-0.309016994374948,0.,0.951056516295154));
#12653=DIRECTION('center_axis',(0.,1.,0.));
#12654=DIRECTION('ref_axis',(1.,0.,0.));
#12655=DIRECTION('center_axis',(0.,1.,0.));
#12656=DIRECTION('ref_axis',(-0.587785252292473,0.,0.809016994374947));
#12657=DIRECTION('center_axis',(0.,1.,0.));
#12658=DIRECTION('ref_axis',(1.,0.,0.));
#12659=DIRECTION('center_axis',(0.,1.,0.));
#12660=DIRECTION('ref_axis',(-0.809016994374947,0.,0.587785252292473));
#12661=DIRECTION('center_axis',(0.,1.,0.));
#12662=DIRECTION('ref_axis',(1.,0.,0.));
#12663=DIRECTION('center_axis',(0.,1.,0.));
#12664=DIRECTION('ref_axis',(-0.951056516295154,0.,0.309016994374947));
#12665=DIRECTION('center_axis',(0.,1.,0.));
#12666=DIRECTION('ref_axis',(1.,0.,0.));
#12667=DIRECTION('center_axis',(0.,1.,0.));
#12668=DIRECTION('ref_axis',(-1.,0.,-1.22464679914735E-16));
#12669=DIRECTION('center_axis',(0.,1.,0.));
#12670=DIRECTION('ref_axis',(1.,0.,0.));
#12671=DIRECTION('center_axis',(0.,1.,0.));
#12672=DIRECTION('ref_axis',(-0.951056516295154,0.,-0.309016994374948));
#12673=DIRECTION('center_axis',(0.,1.,0.));
#12674=DIRECTION('ref_axis',(1.,0.,0.));
#12675=DIRECTION('center_axis',(0.,1.,0.));
#12676=DIRECTION('ref_axis',(-0.809016994374947,0.,-0.587785252292473));
#12677=DIRECTION('center_axis',(0.,1.,0.));
#12678=DIRECTION('ref_axis',(1.,0.,0.));
#12679=DIRECTION('center_axis',(0.,1.,0.));
#12680=DIRECTION('ref_axis',(-0.587785252292473,0.,-0.809016994374948));
#12681=DIRECTION('center_axis',(0.,1.,0.));
#12682=DIRECTION('ref_axis',(1.,0.,0.));
#12683=DIRECTION('center_axis',(0.,1.,0.));
#12684=DIRECTION('ref_axis',(-0.309016994374947,0.,-0.951056516295154));
#12685=DIRECTION('center_axis',(0.,1.,0.));
#12686=DIRECTION('ref_axis',(1.,0.,0.));
#12687=DIRECTION('center_axis',(0.,1.,0.));
#12688=DIRECTION('ref_axis',(6.12323399573677E-17,0.,-1.));
#12689=DIRECTION('center_axis',(0.,1.,0.));
#12690=DIRECTION('ref_axis',(1.,0.,0.));
#12691=DIRECTION('center_axis',(0.,1.,0.));
#12692=DIRECTION('ref_axis',(0.309016994374947,0.,-0.951056516295154));
#12693=DIRECTION('center_axis',(0.,1.,0.));
#12694=DIRECTION('ref_axis',(1.,0.,0.));
#12695=DIRECTION('center_axis',(0.,1.,0.));
#12696=DIRECTION('ref_axis',(0.587785252292473,0.,-0.809016994374947));
#12697=DIRECTION('center_axis',(0.,1.,0.));
#12698=DIRECTION('ref_axis',(1.,0.,0.));
#12699=DIRECTION('center_axis',(0.,1.,0.));
#12700=DIRECTION('ref_axis',(0.809016994374947,0.,-0.587785252292473));
#12701=DIRECTION('center_axis',(0.,1.,0.));
#12702=DIRECTION('ref_axis',(1.,0.,0.));
#12703=DIRECTION('center_axis',(0.,1.,0.));
#12704=DIRECTION('ref_axis',(0.951056516295154,0.,-0.309016994374947));
#12705=DIRECTION('center_axis',(0.,1.,0.));
#12706=DIRECTION('ref_axis',(1.,0.,0.));
#12707=DIRECTION('center_axis',(0.,1.,0.));
#12708=DIRECTION('ref_axis',(1.,0.,0.));
#12709=DIRECTION('center_axis',(0.,1.,0.));
#12710=DIRECTION('ref_axis',(1.,0.,0.));
#12711=DIRECTION('center_axis',(0.,-1.,0.));
#12712=DIRECTION('ref_axis',(1.,0.,0.));
#12713=DIRECTION('center_axis',(0.,-1.,0.));
#12714=DIRECTION('ref_axis',(1.,0.,0.));
#12715=DIRECTION('',(0.,1.,0.));
#12716=DIRECTION('center_axis',(0.,1.,0.));
#12717=DIRECTION('ref_axis',(1.,0.,0.));
#12718=DIRECTION('center_axis',(0.,1.,0.));
#12719=DIRECTION('ref_axis',(1.,0.,0.));
#12720=DIRECTION('center_axis',(0.,1.,0.));
#12721=DIRECTION('ref_axis',(1.,0.,0.));
#12722=DIRECTION('center_axis',(0.,-1.,0.));
#12723=DIRECTION('ref_axis',(0.951056516295154,0.,0.309016994374948));
#12724=DIRECTION('center_axis',(0.,1.,0.));
#12725=DIRECTION('ref_axis',(1.,0.,0.));
#12726=DIRECTION('center_axis',(0.,-1.,0.));
#12727=DIRECTION('ref_axis',(1.,0.,0.));
#12728=DIRECTION('center_axis',(0.,1.,0.));
#12729=DIRECTION('ref_axis',(1.,0.,0.));
#12730=DIRECTION('center_axis',(0.,-1.,0.));
#12731=DIRECTION('ref_axis',(0.951056516295154,0.,-0.309016994374947));
#12732=DIRECTION('center_axis',(0.,1.,0.));
#12733=DIRECTION('ref_axis',(1.,0.,0.));
#12734=DIRECTION('center_axis',(0.,-1.,0.));
#12735=DIRECTION('ref_axis',(0.809016994374947,0.,-0.587785252292473));
#12736=DIRECTION('center_axis',(0.,1.,0.));
#12737=DIRECTION('ref_axis',(1.,0.,0.));
#12738=DIRECTION('center_axis',(0.,-1.,0.));
#12739=DIRECTION('ref_axis',(0.587785252292473,0.,-0.809016994374947));
#12740=DIRECTION('center_axis',(0.,1.,0.));
#12741=DIRECTION('ref_axis',(1.,0.,0.));
#12742=DIRECTION('center_axis',(0.,-1.,0.));
#12743=DIRECTION('ref_axis',(0.309016994374947,0.,-0.951056516295154));
#12744=DIRECTION('center_axis',(0.,1.,0.));
#12745=DIRECTION('ref_axis',(1.,0.,0.));
#12746=DIRECTION('center_axis',(0.,-1.,0.));
#12747=DIRECTION('ref_axis',(6.12323399573677E-17,0.,-1.));
#12748=DIRECTION('center_axis',(0.,1.,0.));
#12749=DIRECTION('ref_axis',(1.,0.,0.));
#12750=DIRECTION('center_axis',(0.,-1.,0.));
#12751=DIRECTION('ref_axis',(-0.309016994374947,0.,-0.951056516295154));
#12752=DIRECTION('center_axis',(0.,1.,0.));
#12753=DIRECTION('ref_axis',(1.,0.,0.));
#12754=DIRECTION('center_axis',(0.,-1.,0.));
#12755=DIRECTION('ref_axis',(-0.587785252292473,0.,-0.809016994374948));
#12756=DIRECTION('center_axis',(0.,1.,0.));
#12757=DIRECTION('ref_axis',(1.,0.,0.));
#12758=DIRECTION('center_axis',(0.,-1.,0.));
#12759=DIRECTION('ref_axis',(-0.809016994374947,0.,-0.587785252292473));
#12760=DIRECTION('center_axis',(0.,1.,0.));
#12761=DIRECTION('ref_axis',(1.,0.,0.));
#12762=DIRECTION('center_axis',(0.,-1.,0.));
#12763=DIRECTION('ref_axis',(-0.951056516295154,0.,-0.309016994374948));
#12764=DIRECTION('center_axis',(0.,1.,0.));
#12765=DIRECTION('ref_axis',(1.,0.,0.));
#12766=DIRECTION('center_axis',(0.,-1.,0.));
#12767=DIRECTION('ref_axis',(-1.,0.,-1.22464679914735E-16));
#12768=DIRECTION('center_axis',(0.,1.,0.));
#12769=DIRECTION('ref_axis',(1.,0.,0.));
#12770=DIRECTION('center_axis',(0.,-1.,0.));
#12771=DIRECTION('ref_axis',(-0.951056516295154,0.,0.309016994374947));
#12772=DIRECTION('center_axis',(0.,1.,0.));
#12773=DIRECTION('ref_axis',(1.,0.,0.));
#12774=DIRECTION('center_axis',(0.,-1.,0.));
#12775=DIRECTION('ref_axis',(-0.809016994374947,0.,0.587785252292473));
#12776=DIRECTION('center_axis',(0.,1.,0.));
#12777=DIRECTION('ref_axis',(1.,0.,0.));
#12778=DIRECTION('center_axis',(0.,-1.,0.));
#12779=DIRECTION('ref_axis',(-0.587785252292473,0.,0.809016994374947));
#12780=DIRECTION('center_axis',(0.,1.,0.));
#12781=DIRECTION('ref_axis',(1.,0.,0.));
#12782=DIRECTION('center_axis',(0.,-1.,0.));
#12783=DIRECTION('ref_axis',(-0.309016994374948,0.,0.951056516295154));
#12784=DIRECTION('center_axis',(0.,1.,0.));
#12785=DIRECTION('ref_axis',(1.,0.,0.));
#12786=DIRECTION('center_axis',(0.,-1.,0.));
#12787=DIRECTION('ref_axis',(-1.83697019872103E-16,0.,1.));
#12788=DIRECTION('center_axis',(0.,1.,0.));
#12789=DIRECTION('ref_axis',(1.,0.,0.));
#12790=DIRECTION('center_axis',(0.,-1.,0.));
#12791=DIRECTION('ref_axis',(0.309016994374947,0.,0.951056516295154));
#12792=DIRECTION('center_axis',(0.,1.,0.));
#12793=DIRECTION('ref_axis',(1.,0.,0.));
#12794=DIRECTION('center_axis',(0.,-1.,0.));
#12795=DIRECTION('ref_axis',(0.587785252292473,0.,0.809016994374948));
#12796=DIRECTION('center_axis',(0.,1.,0.));
#12797=DIRECTION('ref_axis',(1.,0.,0.));
#12798=DIRECTION('center_axis',(0.,-1.,0.));
#12799=DIRECTION('ref_axis',(0.809016994374947,0.,0.587785252292473));
#12800=DIRECTION('center_axis',(0.,1.,0.));
#12801=DIRECTION('ref_axis',(1.,0.,0.));
#12802=DIRECTION('center_axis',(0.,1.,0.));
#12803=DIRECTION('ref_axis',(1.,0.,0.));
#12804=DIRECTION('center_axis',(0.,1.,0.));
#12805=DIRECTION('ref_axis',(1.,0.,0.));
#12806=DIRECTION('',(0.,-1.,0.));
#12807=DIRECTION('center_axis',(0.,1.,0.));
#12808=DIRECTION('ref_axis',(1.,0.,0.));
#12809=DIRECTION('center_axis',(0.,1.,0.));
#12810=DIRECTION('ref_axis',(-0.951056516295153,0.,-0.309016994374948));
#12811=DIRECTION('',(0.,-1.,0.));
#12812=DIRECTION('',(0.,1.,0.));
#12813=DIRECTION('center_axis',(0.,1.,0.));
#12814=DIRECTION('ref_axis',(1.,0.,0.));
#12815=DIRECTION('',(0.,-1.,0.));
#12816=DIRECTION('center_axis',(0.,1.,0.));
#12817=DIRECTION('ref_axis',(-0.809016994374947,0.,-0.587785252292473));
#12818=DIRECTION('',(0.,1.,0.));
#12819=DIRECTION('center_axis',(0.,1.,0.));
#12820=DIRECTION('ref_axis',(1.,0.,0.));
#12821=DIRECTION('',(0.,-1.,0.));
#12822=DIRECTION('center_axis',(0.,1.,0.));
#12823=DIRECTION('ref_axis',(-0.587785252292473,0.,-0.809016994374947));
#12824=DIRECTION('',(0.,1.,0.));
#12825=DIRECTION('center_axis',(0.,1.,0.));
#12826=DIRECTION('ref_axis',(1.,0.,0.));
#12827=DIRECTION('',(0.,-1.,0.));
#12828=DIRECTION('center_axis',(0.,1.,0.));
#12829=DIRECTION('ref_axis',(-0.309016994374947,0.,-0.951056516295154));
#12830=DIRECTION('',(0.,1.,0.));
#12831=DIRECTION('center_axis',(0.,1.,0.));
#12832=DIRECTION('ref_axis',(1.,0.,0.));
#12833=DIRECTION('',(0.,-1.,0.));
#12834=DIRECTION('center_axis',(0.,1.,0.));
#12835=DIRECTION('ref_axis',(-1.37927510063224E-16,0.,-1.));
#12836=DIRECTION('',(0.,1.,0.));
#12837=DIRECTION('center_axis',(0.,1.,0.));
#12838=DIRECTION('ref_axis',(1.,0.,0.));
#12839=DIRECTION('',(0.,-1.,0.));
#12840=DIRECTION('center_axis',(0.,1.,0.));
#12841=DIRECTION('ref_axis',(0.309016994374948,0.,-0.951056516295154));
#12842=DIRECTION('',(0.,1.,0.));
#12843=DIRECTION('center_axis',(0.,1.,0.));
#12844=DIRECTION('ref_axis',(1.,0.,0.));
#12845=DIRECTION('',(0.,-1.,0.));
#12846=DIRECTION('center_axis',(0.,1.,0.));
#12847=DIRECTION('ref_axis',(0.587785252292473,0.,-0.809016994374948));
#12848=DIRECTION('',(0.,1.,0.));
#12849=DIRECTION('center_axis',(0.,1.,0.));
#12850=DIRECTION('ref_axis',(1.,0.,0.));
#12851=DIRECTION('',(0.,-1.,0.));
#12852=DIRECTION('center_axis',(0.,1.,0.));
#12853=DIRECTION('ref_axis',(0.809016994374948,0.,-0.587785252292473));
#12854=DIRECTION('',(0.,1.,0.));
#12855=DIRECTION('center_axis',(0.,1.,0.));
#12856=DIRECTION('ref_axis',(1.,0.,0.));
#12857=DIRECTION('',(0.,-1.,0.));
#12858=DIRECTION('center_axis',(0.,1.,0.));
#12859=DIRECTION('ref_axis',(0.951056516295154,0.,-0.309016994374947));
#12860=DIRECTION('',(0.,1.,0.));
#12861=DIRECTION('center_axis',(0.,1.,0.));
#12862=DIRECTION('ref_axis',(1.,0.,0.));
#12863=DIRECTION('',(0.,-1.,0.));
#12864=DIRECTION('center_axis',(0.,1.,0.));
#12865=DIRECTION('ref_axis',(1.,0.,-1.99159850020592E-16));
#12866=DIRECTION('',(0.,1.,0.));
#12867=DIRECTION('center_axis',(0.,1.,0.));
#12868=DIRECTION('ref_axis',(1.,0.,0.));
#12869=DIRECTION('',(0.,-1.,0.));
#12870=DIRECTION('center_axis',(0.,1.,0.));
#12871=DIRECTION('ref_axis',(0.951056516295154,0.,0.309016994374948));
#12872=DIRECTION('',(0.,1.,0.));
#12873=DIRECTION('center_axis',(0.,1.,0.));
#12874=DIRECTION('ref_axis',(1.,0.,0.));
#12875=DIRECTION('',(0.,-1.,0.));
#12876=DIRECTION('center_axis',(0.,1.,0.));
#12877=DIRECTION('ref_axis',(0.809016994374948,0.,0.587785252292473));
#12878=DIRECTION('',(0.,1.,0.));
#12879=DIRECTION('center_axis',(0.,1.,0.));
#12880=DIRECTION('ref_axis',(1.,0.,0.));
#12881=DIRECTION('',(0.,-1.,0.));
#12882=DIRECTION('center_axis',(0.,1.,0.));
#12883=DIRECTION('ref_axis',(0.587785252292473,0.,0.809016994374948));
#12884=DIRECTION('',(0.,1.,0.));
#12885=DIRECTION('center_axis',(0.,1.,0.));
#12886=DIRECTION('ref_axis',(1.,0.,0.));
#12887=DIRECTION('',(0.,-1.,0.));
#12888=DIRECTION('center_axis',(0.,1.,0.));
#12889=DIRECTION('ref_axis',(0.309016994374947,0.,0.951056516295154));
#12890=DIRECTION('',(0.,1.,0.));
#12891=DIRECTION('center_axis',(0.,1.,0.));
#12892=DIRECTION('ref_axis',(1.,0.,0.));
#12893=DIRECTION('',(0.,-1.,0.));
#12894=DIRECTION('center_axis',(0.,1.,0.));
#12895=DIRECTION('ref_axis',(2.6039218997796E-16,0.,1.));
#12896=DIRECTION('',(0.,1.,0.));
#12897=DIRECTION('center_axis',(0.,1.,0.));
#12898=DIRECTION('ref_axis',(1.,0.,0.));
#12899=DIRECTION('',(0.,-1.,0.));
#12900=DIRECTION('center_axis',(0.,1.,0.));
#12901=DIRECTION('ref_axis',(-0.309016994374948,0.,0.951056516295153));
#12902=DIRECTION('',(0.,1.,0.));
#12903=DIRECTION('center_axis',(0.,1.,0.));
#12904=DIRECTION('ref_axis',(1.,0.,0.));
#12905=DIRECTION('',(0.,-1.,0.));
#12906=DIRECTION('center_axis',(0.,1.,0.));
#12907=DIRECTION('ref_axis',(-0.587785252292474,0.,0.809016994374947));
#12908=DIRECTION('',(0.,1.,0.));
#12909=DIRECTION('center_axis',(0.,1.,0.));
#12910=DIRECTION('ref_axis',(1.,0.,0.));
#12911=DIRECTION('',(0.,-1.,0.));
#12912=DIRECTION('center_axis',(0.,1.,0.));
#12913=DIRECTION('ref_axis',(-0.809016994374948,0.,0.587785252292473));
#12914=DIRECTION('',(0.,1.,0.));
#12915=DIRECTION('center_axis',(0.,1.,0.));
#12916=DIRECTION('ref_axis',(1.,0.,0.));
#12917=DIRECTION('',(0.,-1.,0.));
#12918=DIRECTION('center_axis',(0.,1.,0.));
#12919=DIRECTION('ref_axis',(-0.951056516295154,0.,0.309016994374948));
#12920=DIRECTION('',(0.,1.,0.));
#12921=DIRECTION('center_axis',(0.,1.,0.));
#12922=DIRECTION('ref_axis',(1.,0.,0.));
#12923=DIRECTION('',(0.,1.,0.));
#12924=DIRECTION('center_axis',(0.,1.,0.));
#12925=DIRECTION('ref_axis',(-1.,0.,-1.22464679914735E-16));
#12926=DIRECTION('',(0.,-1.,0.));
#12927=DIRECTION('center_axis',(0.,1.,0.));
#12928=DIRECTION('ref_axis',(1.,0.,0.));
#12929=DIRECTION('axis',(0.,0.,1.));
#12930=DIRECTION('refdir',(1.,0.,0.));
#12931=DIRECTION('axis',(0.,0.,1.));
#12932=DIRECTION('refdir',(1.,0.,0.));
#12933=DIRECTION('center_axis',(0.,1.,0.));
#12934=DIRECTION('ref_axis',(1.,0.,0.));
#12935=DIRECTION('center_axis',(0.,1.,0.));
#12936=DIRECTION('ref_axis',(1.,0.,0.));
#12937=DIRECTION('',(0.,1.,0.));
#12938=DIRECTION('center_axis',(0.,1.,0.));
#12939=DIRECTION('ref_axis',(1.,0.,0.));
#12940=DIRECTION('center_axis',(0.,1.,0.));
#12941=DIRECTION('ref_axis',(1.,0.,0.));
#12942=DIRECTION('center_axis',(0.,1.,0.));
#12943=DIRECTION('ref_axis',(1.,0.,0.));
#12944=DIRECTION('center_axis',(0.,1.,0.));
#12945=DIRECTION('ref_axis',(1.,0.,0.));
#12946=DIRECTION('center_axis',(0.,1.,0.));
#12947=DIRECTION('ref_axis',(1.,0.,0.));
#12948=DIRECTION('center_axis',(0.,1.,0.));
#12949=DIRECTION('ref_axis',(1.,0.,0.));
#12950=DIRECTION('center_axis',(0.,1.,0.));
#12951=DIRECTION('ref_axis',(1.,0.,0.));
#12952=DIRECTION('center_axis',(0.,-1.,0.));
#12953=DIRECTION('ref_axis',(1.,0.,0.));
#12954=DIRECTION('center_axis',(0.,1.,0.));
#12955=DIRECTION('ref_axis',(1.,0.,0.));
#12956=DIRECTION('',(0.,-1.,0.));
#12957=DIRECTION('center_axis',(0.,1.,0.));
#12958=DIRECTION('ref_axis',(1.,0.,0.));
#12959=DIRECTION('',(0.,-1.,0.));
#12960=DIRECTION('center_axis',(0.,1.,0.));
#12961=DIRECTION('ref_axis',(1.,0.,0.));
#12962=DIRECTION('center_axis',(0.,1.,0.));
#12963=DIRECTION('ref_axis',(1.,0.,0.));
#12964=DIRECTION('center_axis',(0.,1.,0.));
#12965=DIRECTION('ref_axis',(1.,0.,0.));
#12966=DIRECTION('center_axis',(0.,1.,0.));
#12967=DIRECTION('ref_axis',(1.,0.,0.));
#12968=DIRECTION('',(0.,-1.,0.));
#12969=DIRECTION('center_axis',(0.,1.,0.));
#12970=DIRECTION('ref_axis',(1.,0.,0.));
#12971=DIRECTION('axis',(0.,0.,1.));
#12972=DIRECTION('refdir',(1.,0.,0.));
#12973=DIRECTION('center_axis',(0.,1.,0.));
#12974=DIRECTION('ref_axis',(1.,0.,0.));
#12975=DIRECTION('center_axis',(0.,-1.,0.));
#12976=DIRECTION('ref_axis',(1.,0.,0.));
#12977=DIRECTION('',(0.,-1.,0.));
#12978=DIRECTION('center_axis',(0.,-1.,0.));
#12979=DIRECTION('ref_axis',(1.,0.,0.));
#12980=DIRECTION('center_axis',(0.,1.,0.));
#12981=DIRECTION('ref_axis',(1.,0.,0.));
#12982=DIRECTION('center_axis',(0.,1.,0.));
#12983=DIRECTION('ref_axis',(1.,0.,0.));
#12984=DIRECTION('',(0.,-1.,0.));
#12985=DIRECTION('center_axis',(0.,1.,0.));
#12986=DIRECTION('ref_axis',(1.,0.,0.));
#12987=DIRECTION('center_axis',(0.,1.,0.));
#12988=DIRECTION('ref_axis',(1.,0.,0.));
#12989=DIRECTION('center_axis',(0.,1.,0.));
#12990=DIRECTION('ref_axis',(1.,0.,0.));
#12991=DIRECTION('axis',(0.,0.,1.));
#12992=DIRECTION('refdir',(1.,0.,0.));
#12993=DIRECTION('center_axis',(0.,1.,0.));
#12994=DIRECTION('ref_axis',(1.,0.,0.));
#12995=DIRECTION('center_axis',(0.,-1.,0.));
#12996=DIRECTION('ref_axis',(1.,0.,0.));
#12997=DIRECTION('',(0.,-1.,0.));
#12998=DIRECTION('center_axis',(0.,-1.,0.));
#12999=DIRECTION('ref_axis',(1.,0.,0.));
#13000=DIRECTION('center_axis',(0.,1.,0.));
#13001=DIRECTION('ref_axis',(1.,0.,0.));
#13002=DIRECTION('center_axis',(0.,1.,0.));
#13003=DIRECTION('ref_axis',(1.,0.,0.));
#13004=DIRECTION('',(0.,-1.,0.));
#13005=DIRECTION('center_axis',(0.,1.,0.));
#13006=DIRECTION('ref_axis',(1.,0.,0.));
#13007=DIRECTION('center_axis',(0.,1.,0.));
#13008=DIRECTION('ref_axis',(1.,0.,0.));
#13009=DIRECTION('center_axis',(0.,1.,0.));
#13010=DIRECTION('ref_axis',(1.,0.,0.));
#13011=DIRECTION('axis',(0.,0.,1.));
#13012=DIRECTION('refdir',(1.,0.,0.));
#13013=DIRECTION('center_axis',(0.,0.,1.));
#13014=DIRECTION('ref_axis',(1.,0.,0.));
#13015=DIRECTION('center_axis',(0.,0.,1.));
#13016=DIRECTION('ref_axis',(1.,0.,0.));
#13017=DIRECTION('',(0.,0.,-1.));
#13018=DIRECTION('center_axis',(0.,0.,1.));
#13019=DIRECTION('ref_axis',(1.,0.,0.));
#13020=DIRECTION('center_axis',(0.,0.,1.));
#13021=DIRECTION('ref_axis',(1.,0.,0.));
#13022=DIRECTION('center_axis',(0.,0.,1.));
#13023=DIRECTION('ref_axis',(1.,0.,0.));
#13024=DIRECTION('axis',(0.,0.,1.));
#13025=DIRECTION('refdir',(1.,0.,0.));
#13026=DIRECTION('center_axis',(0.,0.,1.));
#13027=DIRECTION('ref_axis',(1.,0.,0.));
#13028=DIRECTION('center_axis',(0.,0.,1.));
#13029=DIRECTION('ref_axis',(1.,0.,0.));
#13030=DIRECTION('',(0.,0.,-1.));
#13031=DIRECTION('center_axis',(0.,0.,1.));
#13032=DIRECTION('ref_axis',(1.,0.,0.));
#13033=DIRECTION('center_axis',(0.,0.,1.));
#13034=DIRECTION('ref_axis',(1.,0.,0.));
#13035=DIRECTION('center_axis',(0.,0.,1.));
#13036=DIRECTION('ref_axis',(1.,0.,0.));
#13037=DIRECTION('axis',(0.,0.,1.));
#13038=DIRECTION('refdir',(1.,0.,0.));
#13039=DIRECTION('center_axis',(0.,1.,0.));
#13040=DIRECTION('ref_axis',(1.,0.,0.));
#13041=DIRECTION('center_axis',(0.,-1.,0.));
#13042=DIRECTION('ref_axis',(1.,0.,0.));
#13043=DIRECTION('',(0.,-1.,0.));
#13044=DIRECTION('center_axis',(0.,-1.,0.));
#13045=DIRECTION('ref_axis',(1.,0.,0.));
#13046=DIRECTION('center_axis',(0.,1.,0.));
#13047=DIRECTION('ref_axis',(1.,0.,0.));
#13048=DIRECTION('center_axis',(0.,1.,0.));
#13049=DIRECTION('ref_axis',(1.,0.,0.));
#13050=DIRECTION('',(0.,-1.,0.));
#13051=DIRECTION('center_axis',(0.,1.,0.));
#13052=DIRECTION('ref_axis',(1.,0.,0.));
#13053=DIRECTION('center_axis',(0.,1.,0.));
#13054=DIRECTION('ref_axis',(1.,0.,0.));
#13055=DIRECTION('center_axis',(0.,1.,0.));
#13056=DIRECTION('ref_axis',(1.,0.,0.));
#13057=DIRECTION('axis',(0.,0.,1.));
#13058=DIRECTION('refdir',(1.,0.,0.));
#13059=DIRECTION('center_axis',(1.,0.,6.12323399573677E-17));
#13060=DIRECTION('ref_axis',(6.12323399573677E-17,0.,-1.));
#13061=DIRECTION('',(1.,0.,6.12323399573677E-17));
#13062=DIRECTION('center_axis',(1.,0.,6.12323399573677E-17));
#13063=DIRECTION('ref_axis',(6.12323399573677E-17,0.,-1.));
#13064=DIRECTION('',(1.,0.,6.12323399573677E-17));
#13065=DIRECTION('center_axis',(0.,-1.,0.));
#13066=DIRECTION('ref_axis',(1.,0.,0.));
#13067=DIRECTION('center_axis',(0.,-1.,0.));
#13068=DIRECTION('ref_axis',(1.,0.,0.));
#13069=DIRECTION('',(0.,1.,0.));
#13070=DIRECTION('',(0.,1.,0.));
#13071=DIRECTION('center_axis',(0.,1.,0.));
#13072=DIRECTION('ref_axis',(1.,0.,0.));
#13073=DIRECTION('center_axis',(0.,0.,1.));
#13074=DIRECTION('ref_axis',(1.,0.,0.));
#13075=DIRECTION('',(0.,0.,1.));
#13076=DIRECTION('center_axis',(0.,0.,1.));
#13077=DIRECTION('ref_axis',(1.,0.,0.));
#13078=DIRECTION('',(0.,0.,1.));
#13079=DIRECTION('center_axis',(0.,1.,0.));
#13080=DIRECTION('ref_axis',(1.,0.,0.));
#13081=DIRECTION('center_axis',(0.,1.,0.));
#13082=DIRECTION('ref_axis',(1.,0.,0.));
#13083=DIRECTION('',(0.,1.,0.));
#13084=DIRECTION('',(0.,1.,0.));
#13085=DIRECTION('center_axis',(0.,-1.,0.));
#13086=DIRECTION('ref_axis',(1.,0.,0.));
#13087=DIRECTION('center_axis',(0.,1.,0.));
#13088=DIRECTION('ref_axis',(1.,0.,0.));
#13089=DIRECTION('center_axis',(0.,1.,0.));
#13090=DIRECTION('ref_axis',(1.,0.,0.));
#13091=DIRECTION('center_axis',(0.,1.,0.));
#13092=DIRECTION('ref_axis',(1.,0.,0.));
#13093=DIRECTION('center_axis',(0.,1.,0.));
#13094=DIRECTION('ref_axis',(0.987688340595138,0.,0.156434465040231));
#13095=DIRECTION('center_axis',(0.,1.,0.));
#13096=DIRECTION('ref_axis',(1.,0.,0.));
#13097=DIRECTION('center_axis',(0.,1.,0.));
#13098=DIRECTION('ref_axis',(0.951056516295154,0.,0.309016994374948));
#13099=DIRECTION('center_axis',(0.,1.,0.));
#13100=DIRECTION('ref_axis',(1.,0.,0.));
#13101=DIRECTION('center_axis',(0.,1.,0.));
#13102=DIRECTION('ref_axis',(0.891006524188368,0.,0.453990499739547));
#13103=DIRECTION('center_axis',(0.,1.,0.));
#13104=DIRECTION('ref_axis',(1.,0.,0.));
#13105=DIRECTION('center_axis',(0.,1.,0.));
#13106=DIRECTION('ref_axis',(0.809016994374947,0.,0.587785252292473));
#13107=DIRECTION('center_axis',(0.,1.,0.));
#13108=DIRECTION('ref_axis',(1.,0.,0.));
#13109=DIRECTION('center_axis',(0.,1.,0.));
#13110=DIRECTION('ref_axis',(0.707106781186547,0.,0.707106781186548));
#13111=DIRECTION('center_axis',(0.,1.,0.));
#13112=DIRECTION('ref_axis',(1.,0.,0.));
#13113=DIRECTION('center_axis',(0.,1.,0.));
#13114=DIRECTION('ref_axis',(0.587785252292473,0.,0.809016994374948));
#13115=DIRECTION('center_axis',(0.,1.,0.));
#13116=DIRECTION('ref_axis',(1.,0.,0.));
#13117=DIRECTION('center_axis',(0.,1.,0.));
#13118=DIRECTION('ref_axis',(0.453990499739547,0.,0.891006524188368));
#13119=DIRECTION('center_axis',(0.,1.,0.));
#13120=DIRECTION('ref_axis',(1.,0.,0.));
#13121=DIRECTION('center_axis',(0.,1.,0.));
#13122=DIRECTION('ref_axis',(0.309016994374947,0.,0.951056516295154));
#13123=DIRECTION('center_axis',(0.,1.,0.));
#13124=DIRECTION('ref_axis',(1.,0.,0.));
#13125=DIRECTION('center_axis',(0.,1.,0.));
#13126=DIRECTION('ref_axis',(0.156434465040231,0.,0.987688340595138));
#13127=DIRECTION('center_axis',(0.,1.,0.));
#13128=DIRECTION('ref_axis',(1.,0.,0.));
#13129=DIRECTION('center_axis',(0.,1.,0.));
#13130=DIRECTION('ref_axis',(-1.83697019872103E-16,0.,1.));
#13131=DIRECTION('center_axis',(0.,1.,0.));
#13132=DIRECTION('ref_axis',(1.,0.,0.));
#13133=DIRECTION('center_axis',(0.,1.,0.));
#13134=DIRECTION('ref_axis',(-0.156434465040231,0.,0.987688340595138));
#13135=DIRECTION('center_axis',(0.,1.,0.));
#13136=DIRECTION('ref_axis',(1.,0.,0.));
#13137=DIRECTION('center_axis',(0.,1.,0.));
#13138=DIRECTION('ref_axis',(-0.309016994374948,0.,0.951056516295154));
#13139=DIRECTION('center_axis',(0.,1.,0.));
#13140=DIRECTION('ref_axis',(1.,0.,0.));
#13141=DIRECTION('center_axis',(0.,1.,0.));
#13142=DIRECTION('ref_axis',(-0.453990499739547,0.,0.891006524188368));
#13143=DIRECTION('center_axis',(0.,1.,0.));
#13144=DIRECTION('ref_axis',(1.,0.,0.));
#13145=DIRECTION('center_axis',(0.,1.,0.));
#13146=DIRECTION('ref_axis',(-0.587785252292473,0.,0.809016994374947));
#13147=DIRECTION('center_axis',(0.,1.,0.));
#13148=DIRECTION('ref_axis',(1.,0.,0.));
#13149=DIRECTION('center_axis',(0.,1.,0.));
#13150=DIRECTION('ref_axis',(-0.707106781186548,0.,0.707106781186547));
#13151=DIRECTION('center_axis',(0.,1.,0.));
#13152=DIRECTION('ref_axis',(1.,0.,0.));
#13153=DIRECTION('center_axis',(0.,1.,0.));
#13154=DIRECTION('ref_axis',(-0.809016994374947,0.,0.587785252292473));
#13155=DIRECTION('center_axis',(0.,1.,0.));
#13156=DIRECTION('ref_axis',(1.,0.,0.));
#13157=DIRECTION('center_axis',(0.,1.,0.));
#13158=DIRECTION('ref_axis',(-0.891006524188368,0.,0.453990499739547));
#13159=DIRECTION('center_axis',(0.,1.,0.));
#13160=DIRECTION('ref_axis',(1.,0.,0.));
#13161=DIRECTION('center_axis',(0.,1.,0.));
#13162=DIRECTION('ref_axis',(-0.951056516295154,0.,0.309016994374947));
#13163=DIRECTION('center_axis',(0.,1.,0.));
#13164=DIRECTION('ref_axis',(1.,0.,0.));
#13165=DIRECTION('center_axis',(0.,1.,0.));
#13166=DIRECTION('ref_axis',(-0.987688340595138,0.,0.156434465040231));
#13167=DIRECTION('center_axis',(0.,1.,0.));
#13168=DIRECTION('ref_axis',(1.,0.,0.));
#13169=DIRECTION('center_axis',(0.,1.,0.));
#13170=DIRECTION('ref_axis',(-1.,0.,-1.22464679914735E-16));
#13171=DIRECTION('center_axis',(0.,1.,0.));
#13172=DIRECTION('ref_axis',(1.,0.,0.));
#13173=DIRECTION('center_axis',(0.,1.,0.));
#13174=DIRECTION('ref_axis',(-0.987688340595138,0.,-0.156434465040231));
#13175=DIRECTION('center_axis',(0.,1.,0.));
#13176=DIRECTION('ref_axis',(1.,0.,0.));
#13177=DIRECTION('center_axis',(0.,1.,0.));
#13178=DIRECTION('ref_axis',(-0.951056516295154,0.,-0.309016994374948));
#13179=DIRECTION('center_axis',(0.,1.,0.));
#13180=DIRECTION('ref_axis',(1.,0.,0.));
#13181=DIRECTION('center_axis',(0.,1.,0.));
#13182=DIRECTION('ref_axis',(-0.891006524188368,0.,-0.453990499739547));
#13183=DIRECTION('center_axis',(0.,1.,0.));
#13184=DIRECTION('ref_axis',(1.,0.,0.));
#13185=DIRECTION('center_axis',(0.,1.,0.));
#13186=DIRECTION('ref_axis',(-0.809016994374947,0.,-0.587785252292473));
#13187=DIRECTION('center_axis',(0.,1.,0.));
#13188=DIRECTION('ref_axis',(1.,0.,0.));
#13189=DIRECTION('center_axis',(0.,1.,0.));
#13190=DIRECTION('ref_axis',(-0.707106781186547,0.,-0.707106781186548));
#13191=DIRECTION('center_axis',(0.,1.,0.));
#13192=DIRECTION('ref_axis',(1.,0.,0.));
#13193=DIRECTION('center_axis',(0.,1.,0.));
#13194=DIRECTION('ref_axis',(-0.587785252292473,0.,-0.809016994374947));
#13195=DIRECTION('center_axis',(0.,1.,0.));
#13196=DIRECTION('ref_axis',(1.,0.,0.));
#13197=DIRECTION('center_axis',(0.,1.,0.));
#13198=DIRECTION('ref_axis',(-0.453990499739547,0.,-0.891006524188368));
#13199=DIRECTION('center_axis',(0.,1.,0.));
#13200=DIRECTION('ref_axis',(1.,0.,0.));
#13201=DIRECTION('center_axis',(0.,1.,0.));
#13202=DIRECTION('ref_axis',(-0.309016994374947,0.,-0.951056516295154));
#13203=DIRECTION('center_axis',(0.,1.,0.));
#13204=DIRECTION('ref_axis',(1.,0.,0.));
#13205=DIRECTION('center_axis',(0.,1.,0.));
#13206=DIRECTION('ref_axis',(-0.156434465040231,0.,-0.987688340595138));
#13207=DIRECTION('center_axis',(0.,1.,0.));
#13208=DIRECTION('ref_axis',(1.,0.,0.));
#13209=DIRECTION('center_axis',(0.,1.,0.));
#13210=DIRECTION('ref_axis',(6.12323399573677E-17,0.,-1.));
#13211=DIRECTION('center_axis',(0.,1.,0.));
#13212=DIRECTION('ref_axis',(1.,0.,0.));
#13213=DIRECTION('center_axis',(0.,1.,0.));
#13214=DIRECTION('ref_axis',(0.156434465040231,0.,-0.987688340595138));
#13215=DIRECTION('center_axis',(0.,1.,0.));
#13216=DIRECTION('ref_axis',(1.,0.,0.));
#13217=DIRECTION('center_axis',(0.,1.,0.));
#13218=DIRECTION('ref_axis',(0.309016994374948,0.,-0.951056516295154));
#13219=DIRECTION('center_axis',(0.,1.,0.));
#13220=DIRECTION('ref_axis',(1.,0.,0.));
#13221=DIRECTION('center_axis',(0.,1.,0.));
#13222=DIRECTION('ref_axis',(0.453990499739547,0.,-0.891006524188368));
#13223=DIRECTION('center_axis',(0.,1.,0.));
#13224=DIRECTION('ref_axis',(1.,0.,0.));
#13225=DIRECTION('center_axis',(0.,1.,0.));
#13226=DIRECTION('ref_axis',(0.587785252292473,0.,-0.809016994374947));
#13227=DIRECTION('center_axis',(0.,1.,0.));
#13228=DIRECTION('ref_axis',(1.,0.,0.));
#13229=DIRECTION('center_axis',(0.,1.,0.));
#13230=DIRECTION('ref_axis',(0.707106781186548,0.,-0.707106781186547));
#13231=DIRECTION('center_axis',(0.,1.,0.));
#13232=DIRECTION('ref_axis',(1.,0.,0.));
#13233=DIRECTION('center_axis',(0.,1.,0.));
#13234=DIRECTION('ref_axis',(0.809016994374947,0.,-0.587785252292473));
#13235=DIRECTION('center_axis',(0.,1.,0.));
#13236=DIRECTION('ref_axis',(1.,0.,0.));
#13237=DIRECTION('center_axis',(0.,1.,0.));
#13238=DIRECTION('ref_axis',(0.891006524188368,0.,-0.453990499739547));
#13239=DIRECTION('center_axis',(0.,1.,0.));
#13240=DIRECTION('ref_axis',(1.,0.,0.));
#13241=DIRECTION('center_axis',(0.,1.,0.));
#13242=DIRECTION('ref_axis',(0.951056516295154,0.,-0.309016994374947));
#13243=DIRECTION('center_axis',(0.,1.,0.));
#13244=DIRECTION('ref_axis',(1.,0.,0.));
#13245=DIRECTION('center_axis',(0.,1.,0.));
#13246=DIRECTION('ref_axis',(0.987688340595138,0.,-0.156434465040231));
#13247=DIRECTION('center_axis',(0.,1.,0.));
#13248=DIRECTION('ref_axis',(1.,0.,0.));
#13249=DIRECTION('center_axis',(0.,1.,0.));
#13250=DIRECTION('ref_axis',(1.,0.,0.));
#13251=DIRECTION('center_axis',(0.,1.,0.));
#13252=DIRECTION('ref_axis',(1.,0.,0.));
#13253=DIRECTION('center_axis',(0.,-1.,0.));
#13254=DIRECTION('ref_axis',(1.,0.,0.));
#13255=DIRECTION('center_axis',(0.,-1.,0.));
#13256=DIRECTION('ref_axis',(1.,0.,0.));
#13257=DIRECTION('',(0.,1.,0.));
#13258=DIRECTION('center_axis',(0.,1.,0.));
#13259=DIRECTION('ref_axis',(1.,0.,0.));
#13260=DIRECTION('center_axis',(0.,1.,0.));
#13261=DIRECTION('ref_axis',(1.,0.,0.));
#13262=DIRECTION('center_axis',(0.,1.,0.));
#13263=DIRECTION('ref_axis',(1.,0.,0.));
#13264=DIRECTION('center_axis',(0.,-1.,0.));
#13265=DIRECTION('ref_axis',(0.987688340595138,0.,0.156434465040231));
#13266=DIRECTION('center_axis',(0.,1.,0.));
#13267=DIRECTION('ref_axis',(1.,0.,0.));
#13268=DIRECTION('center_axis',(0.,-1.,0.));
#13269=DIRECTION('ref_axis',(1.,0.,0.));
#13270=DIRECTION('center_axis',(0.,1.,0.));
#13271=DIRECTION('ref_axis',(1.,0.,0.));
#13272=DIRECTION('center_axis',(0.,-1.,0.));
#13273=DIRECTION('ref_axis',(0.987688340595138,0.,-0.156434465040231));
#13274=DIRECTION('center_axis',(0.,1.,0.));
#13275=DIRECTION('ref_axis',(1.,0.,0.));
#13276=DIRECTION('center_axis',(0.,-1.,0.));
#13277=DIRECTION('ref_axis',(0.951056516295154,0.,-0.309016994374947));
#13278=DIRECTION('center_axis',(0.,1.,0.));
#13279=DIRECTION('ref_axis',(1.,0.,0.));
#13280=DIRECTION('center_axis',(0.,-1.,0.));
#13281=DIRECTION('ref_axis',(0.891006524188368,0.,-0.453990499739547));
#13282=DIRECTION('center_axis',(0.,1.,0.));
#13283=DIRECTION('ref_axis',(1.,0.,0.));
#13284=DIRECTION('center_axis',(0.,-1.,0.));
#13285=DIRECTION('ref_axis',(0.809016994374947,0.,-0.587785252292473));
#13286=DIRECTION('center_axis',(0.,1.,0.));
#13287=DIRECTION('ref_axis',(1.,0.,0.));
#13288=DIRECTION('center_axis',(0.,-1.,0.));
#13289=DIRECTION('ref_axis',(0.707106781186548,0.,-0.707106781186547));
#13290=DIRECTION('center_axis',(0.,1.,0.));
#13291=DIRECTION('ref_axis',(1.,0.,0.));
#13292=DIRECTION('center_axis',(0.,-1.,0.));
#13293=DIRECTION('ref_axis',(0.587785252292473,0.,-0.809016994374947));
#13294=DIRECTION('center_axis',(0.,1.,0.));
#13295=DIRECTION('ref_axis',(1.,0.,0.));
#13296=DIRECTION('center_axis',(0.,-1.,0.));
#13297=DIRECTION('ref_axis',(0.453990499739547,0.,-0.891006524188368));
#13298=DIRECTION('center_axis',(0.,1.,0.));
#13299=DIRECTION('ref_axis',(1.,0.,0.));
#13300=DIRECTION('center_axis',(0.,-1.,0.));
#13301=DIRECTION('ref_axis',(0.309016994374948,0.,-0.951056516295154));
#13302=DIRECTION('center_axis',(0.,1.,0.));
#13303=DIRECTION('ref_axis',(1.,0.,0.));
#13304=DIRECTION('center_axis',(0.,-1.,0.));
#13305=DIRECTION('ref_axis',(0.156434465040231,0.,-0.987688340595138));
#13306=DIRECTION('center_axis',(0.,1.,0.));
#13307=DIRECTION('ref_axis',(1.,0.,0.));
#13308=DIRECTION('center_axis',(0.,-1.,0.));
#13309=DIRECTION('ref_axis',(6.12323399573677E-17,0.,-1.));
#13310=DIRECTION('center_axis',(0.,1.,0.));
#13311=DIRECTION('ref_axis',(1.,0.,0.));
#13312=DIRECTION('center_axis',(0.,-1.,0.));
#13313=DIRECTION('ref_axis',(-0.156434465040231,0.,-0.987688340595138));
#13314=DIRECTION('center_axis',(0.,1.,0.));
#13315=DIRECTION('ref_axis',(1.,0.,0.));
#13316=DIRECTION('center_axis',(0.,-1.,0.));
#13317=DIRECTION('ref_axis',(-0.309016994374947,0.,-0.951056516295154));
#13318=DIRECTION('center_axis',(0.,1.,0.));
#13319=DIRECTION('ref_axis',(1.,0.,0.));
#13320=DIRECTION('center_axis',(0.,-1.,0.));
#13321=DIRECTION('ref_axis',(-0.453990499739547,0.,-0.891006524188368));
#13322=DIRECTION('center_axis',(0.,1.,0.));
#13323=DIRECTION('ref_axis',(1.,0.,0.));
#13324=DIRECTION('center_axis',(0.,-1.,0.));
#13325=DIRECTION('ref_axis',(-0.587785252292473,0.,-0.809016994374947));
#13326=DIRECTION('center_axis',(0.,1.,0.));
#13327=DIRECTION('ref_axis',(1.,0.,0.));
#13328=DIRECTION('center_axis',(0.,-1.,0.));
#13329=DIRECTION('ref_axis',(-0.707106781186547,0.,-0.707106781186548));
#13330=DIRECTION('center_axis',(0.,1.,0.));
#13331=DIRECTION('ref_axis',(1.,0.,0.));
#13332=DIRECTION('center_axis',(0.,-1.,0.));
#13333=DIRECTION('ref_axis',(-0.809016994374947,0.,-0.587785252292473));
#13334=DIRECTION('center_axis',(0.,1.,0.));
#13335=DIRECTION('ref_axis',(1.,0.,0.));
#13336=DIRECTION('center_axis',(0.,-1.,0.));
#13337=DIRECTION('ref_axis',(-0.891006524188368,0.,-0.453990499739547));
#13338=DIRECTION('center_axis',(0.,1.,0.));
#13339=DIRECTION('ref_axis',(1.,0.,0.));
#13340=DIRECTION('center_axis',(0.,-1.,0.));
#13341=DIRECTION('ref_axis',(-0.951056516295154,0.,-0.309016994374948));
#13342=DIRECTION('center_axis',(0.,1.,0.));
#13343=DIRECTION('ref_axis',(1.,0.,0.));
#13344=DIRECTION('center_axis',(0.,-1.,0.));
#13345=DIRECTION('ref_axis',(-0.987688340595138,0.,-0.156434465040231));
#13346=DIRECTION('center_axis',(0.,1.,0.));
#13347=DIRECTION('ref_axis',(1.,0.,0.));
#13348=DIRECTION('center_axis',(0.,-1.,0.));
#13349=DIRECTION('ref_axis',(-1.,0.,-1.22464679914735E-16));
#13350=DIRECTION('center_axis',(0.,1.,0.));
#13351=DIRECTION('ref_axis',(1.,0.,0.));
#13352=DIRECTION('center_axis',(0.,-1.,0.));
#13353=DIRECTION('ref_axis',(-0.987688340595138,0.,0.156434465040231));
#13354=DIRECTION('center_axis',(0.,1.,0.));
#13355=DIRECTION('ref_axis',(1.,0.,0.));
#13356=DIRECTION('center_axis',(0.,-1.,0.));
#13357=DIRECTION('ref_axis',(-0.951056516295154,0.,0.309016994374947));
#13358=DIRECTION('center_axis',(0.,1.,0.));
#13359=DIRECTION('ref_axis',(1.,0.,0.));
#13360=DIRECTION('center_axis',(0.,-1.,0.));
#13361=DIRECTION('ref_axis',(-0.891006524188368,0.,0.453990499739547));
#13362=DIRECTION('center_axis',(0.,1.,0.));
#13363=DIRECTION('ref_axis',(1.,0.,0.));
#13364=DIRECTION('center_axis',(0.,-1.,0.));
#13365=DIRECTION('ref_axis',(-0.809016994374947,0.,0.587785252292473));
#13366=DIRECTION('center_axis',(0.,1.,0.));
#13367=DIRECTION('ref_axis',(1.,0.,0.));
#13368=DIRECTION('center_axis',(0.,-1.,0.));
#13369=DIRECTION('ref_axis',(-0.707106781186548,0.,0.707106781186547));
#13370=DIRECTION('center_axis',(0.,1.,0.));
#13371=DIRECTION('ref_axis',(1.,0.,0.));
#13372=DIRECTION('center_axis',(0.,-1.,0.));
#13373=DIRECTION('ref_axis',(-0.587785252292473,0.,0.809016994374947));
#13374=DIRECTION('center_axis',(0.,1.,0.));
#13375=DIRECTION('ref_axis',(1.,0.,0.));
#13376=DIRECTION('center_axis',(0.,-1.,0.));
#13377=DIRECTION('ref_axis',(-0.453990499739547,0.,0.891006524188368));
#13378=DIRECTION('center_axis',(0.,1.,0.));
#13379=DIRECTION('ref_axis',(1.,0.,0.));
#13380=DIRECTION('center_axis',(0.,-1.,0.));
#13381=DIRECTION('ref_axis',(-0.309016994374948,0.,0.951056516295154));
#13382=DIRECTION('center_axis',(0.,1.,0.));
#13383=DIRECTION('ref_axis',(1.,0.,0.));
#13384=DIRECTION('center_axis',(0.,-1.,0.));
#13385=DIRECTION('ref_axis',(-0.156434465040231,0.,0.987688340595138));
#13386=DIRECTION('center_axis',(0.,1.,0.));
#13387=DIRECTION('ref_axis',(1.,0.,0.));
#13388=DIRECTION('center_axis',(0.,-1.,0.));
#13389=DIRECTION('ref_axis',(-1.83697019872103E-16,0.,1.));
#13390=DIRECTION('center_axis',(0.,1.,0.));
#13391=DIRECTION('ref_axis',(1.,0.,0.));
#13392=DIRECTION('center_axis',(0.,-1.,0.));
#13393=DIRECTION('ref_axis',(0.156434465040231,0.,0.987688340595138));
#13394=DIRECTION('center_axis',(0.,1.,0.));
#13395=DIRECTION('ref_axis',(1.,0.,0.));
#13396=DIRECTION('center_axis',(0.,-1.,0.));
#13397=DIRECTION('ref_axis',(0.309016994374947,0.,0.951056516295154));
#13398=DIRECTION('center_axis',(0.,1.,0.));
#13399=DIRECTION('ref_axis',(1.,0.,0.));
#13400=DIRECTION('center_axis',(0.,-1.,0.));
#13401=DIRECTION('ref_axis',(0.453990499739547,0.,0.891006524188368));
#13402=DIRECTION('center_axis',(0.,1.,0.));
#13403=DIRECTION('ref_axis',(1.,0.,0.));
#13404=DIRECTION('center_axis',(0.,-1.,0.));
#13405=DIRECTION('ref_axis',(0.587785252292473,0.,0.809016994374948));
#13406=DIRECTION('center_axis',(0.,1.,0.));
#13407=DIRECTION('ref_axis',(1.,0.,0.));
#13408=DIRECTION('center_axis',(0.,-1.,0.));
#13409=DIRECTION('ref_axis',(0.707106781186547,0.,0.707106781186548));
#13410=DIRECTION('center_axis',(0.,1.,0.));
#13411=DIRECTION('ref_axis',(1.,0.,0.));
#13412=DIRECTION('center_axis',(0.,-1.,0.));
#13413=DIRECTION('ref_axis',(0.809016994374947,0.,0.587785252292473));
#13414=DIRECTION('center_axis',(0.,1.,0.));
#13415=DIRECTION('ref_axis',(1.,0.,0.));
#13416=DIRECTION('center_axis',(0.,-1.,0.));
#13417=DIRECTION('ref_axis',(0.891006524188368,0.,0.453990499739547));
#13418=DIRECTION('center_axis',(0.,1.,0.));
#13419=DIRECTION('ref_axis',(1.,0.,0.));
#13420=DIRECTION('center_axis',(0.,-1.,0.));
#13421=DIRECTION('ref_axis',(0.951056516295154,0.,0.309016994374948));
#13422=DIRECTION('center_axis',(0.,1.,0.));
#13423=DIRECTION('ref_axis',(1.,0.,0.));
#13424=DIRECTION('center_axis',(0.,1.,0.));
#13425=DIRECTION('ref_axis',(1.,0.,0.));
#13426=DIRECTION('center_axis',(0.,1.,0.));
#13427=DIRECTION('ref_axis',(1.,0.,0.));
#13428=DIRECTION('',(0.,-1.,0.));
#13429=DIRECTION('center_axis',(0.,1.,0.));
#13430=DIRECTION('ref_axis',(1.,0.,0.));
#13431=DIRECTION('center_axis',(0.,1.,0.));
#13432=DIRECTION('ref_axis',(-0.987688340595137,0.,-0.156434465040233));
#13433=DIRECTION('',(0.,-1.,0.));
#13434=DIRECTION('',(0.,1.,0.));
#13435=DIRECTION('center_axis',(0.,1.,0.));
#13436=DIRECTION('ref_axis',(1.,0.,0.));
#13437=DIRECTION('',(0.,-1.,0.));
#13438=DIRECTION('center_axis',(0.,1.,0.));
#13439=DIRECTION('ref_axis',(-0.951056516295153,0.,-0.309016994374949));
#13440=DIRECTION('',(0.,1.,0.));
#13441=DIRECTION('center_axis',(0.,1.,0.));
#13442=DIRECTION('ref_axis',(1.,0.,0.));
#13443=DIRECTION('',(0.,-1.,0.));
#13444=DIRECTION('center_axis',(0.,1.,0.));
#13445=DIRECTION('ref_axis',(-0.891006524188368,0.,-0.453990499739547));
#13446=DIRECTION('',(0.,1.,0.));
#13447=DIRECTION('center_axis',(0.,1.,0.));
#13448=DIRECTION('ref_axis',(1.,0.,0.));
#13449=DIRECTION('',(0.,-1.,0.));
#13450=DIRECTION('center_axis',(0.,1.,0.));
#13451=DIRECTION('ref_axis',(-0.809016994374948,0.,-0.587785252292473));
#13452=DIRECTION('',(0.,1.,0.));
#13453=DIRECTION('center_axis',(0.,1.,0.));
#13454=DIRECTION('ref_axis',(1.,0.,0.));
#13455=DIRECTION('',(0.,-1.,0.));
#13456=DIRECTION('center_axis',(0.,1.,0.));
#13457=DIRECTION('ref_axis',(-0.707106781186547,0.,-0.707106781186548));
#13458=DIRECTION('',(0.,1.,0.));
#13459=DIRECTION('center_axis',(0.,1.,0.));
#13460=DIRECTION('ref_axis',(1.,0.,0.));
#13461=DIRECTION('',(0.,-1.,0.));
#13462=DIRECTION('center_axis',(0.,1.,0.));
#13463=DIRECTION('ref_axis',(-0.587785252292474,0.,-0.809016994374947));
#13464=DIRECTION('',(0.,1.,0.));
#13465=DIRECTION('center_axis',(0.,1.,0.));
#13466=DIRECTION('ref_axis',(1.,0.,0.));
#13467=DIRECTION('',(0.,-1.,0.));
#13468=DIRECTION('center_axis',(0.,1.,0.));
#13469=DIRECTION('ref_axis',(-0.453990499739547,0.,-0.891006524188368));
#13470=DIRECTION('',(0.,1.,0.));
#13471=DIRECTION('center_axis',(0.,1.,0.));
#13472=DIRECTION('ref_axis',(1.,0.,0.));
#13473=DIRECTION('',(0.,-1.,0.));
#13474=DIRECTION('center_axis',(0.,1.,0.));
#13475=DIRECTION('ref_axis',(-0.309016994374948,0.,-0.951056516295153));
#13476=DIRECTION('',(0.,1.,0.));
#13477=DIRECTION('center_axis',(0.,1.,0.));
#13478=DIRECTION('ref_axis',(1.,0.,0.));
#13479=DIRECTION('',(0.,-1.,0.));
#13480=DIRECTION('center_axis',(0.,1.,0.));
#13481=DIRECTION('ref_axis',(-0.156434465040232,0.,-0.987688340595138));
#13482=DIRECTION('',(0.,1.,0.));
#13483=DIRECTION('center_axis',(0.,1.,0.));
#13484=DIRECTION('ref_axis',(1.,0.,0.));
#13485=DIRECTION('',(0.,-1.,0.));
#13486=DIRECTION('center_axis',(0.,1.,0.));
#13487=DIRECTION('ref_axis',(3.06161699786838E-16,0.,-1.));
#13488=DIRECTION('',(0.,1.,0.));
#13489=DIRECTION('center_axis',(0.,1.,0.));
#13490=DIRECTION('ref_axis',(1.,0.,0.));
#13491=DIRECTION('',(0.,-1.,0.));
#13492=DIRECTION('center_axis',(0.,1.,0.));
#13493=DIRECTION('ref_axis',(0.156434465040233,0.,-0.987688340595138));
#13494=DIRECTION('',(0.,1.,0.));
#13495=DIRECTION('center_axis',(0.,1.,0.));
#13496=DIRECTION('ref_axis',(1.,0.,0.));
#13497=DIRECTION('',(0.,-1.,0.));
#13498=DIRECTION('center_axis',(0.,1.,0.));
#13499=DIRECTION('ref_axis',(0.309016994374946,0.,-0.951056516295154));
#13500=DIRECTION('',(0.,1.,0.));
#13501=DIRECTION('center_axis',(0.,1.,0.));
#13502=DIRECTION('ref_axis',(1.,0.,0.));
#13503=DIRECTION('',(0.,-1.,0.));
#13504=DIRECTION('center_axis',(0.,1.,0.));
#13505=DIRECTION('ref_axis',(0.453990499739547,0.,-0.891006524188368));
#13506=DIRECTION('',(0.,1.,0.));
#13507=DIRECTION('center_axis',(0.,1.,0.));
#13508=DIRECTION('ref_axis',(1.,0.,0.));
#13509=DIRECTION('',(0.,-1.,0.));
#13510=DIRECTION('center_axis',(0.,1.,0.));
#13511=DIRECTION('ref_axis',(0.587785252292473,0.,-0.809016994374947));
#13512=DIRECTION('',(0.,1.,0.));
#13513=DIRECTION('center_axis',(0.,1.,0.));
#13514=DIRECTION('ref_axis',(1.,0.,0.));
#13515=DIRECTION('',(0.,-1.,0.));
#13516=DIRECTION('center_axis',(0.,1.,0.));
#13517=DIRECTION('ref_axis',(0.707106781186548,0.,-0.707106781186547));
#13518=DIRECTION('',(0.,1.,0.));
#13519=DIRECTION('center_axis',(0.,1.,0.));
#13520=DIRECTION('ref_axis',(1.,0.,0.));
#13521=DIRECTION('',(0.,-1.,0.));
#13522=DIRECTION('center_axis',(0.,1.,0.));
#13523=DIRECTION('ref_axis',(0.809016994374946,0.,-0.587785252292475));
#13524=DIRECTION('',(0.,1.,0.));
#13525=DIRECTION('center_axis',(0.,1.,0.));
#13526=DIRECTION('ref_axis',(1.,0.,0.));
#13527=DIRECTION('',(0.,-1.,0.));
#13528=DIRECTION('center_axis',(0.,1.,0.));
#13529=DIRECTION('ref_axis',(0.891006524188368,0.,-0.453990499739547));
#13530=DIRECTION('',(0.,1.,0.));
#13531=DIRECTION('center_axis',(0.,1.,0.));
#13532=DIRECTION('ref_axis',(1.,0.,0.));
#13533=DIRECTION('',(0.,-1.,0.));
#13534=DIRECTION('center_axis',(0.,1.,0.));
#13535=DIRECTION('ref_axis',(0.951056516295154,0.,-0.309016994374946));
#13536=DIRECTION('',(0.,1.,0.));
#13537=DIRECTION('center_axis',(0.,1.,0.));
#13538=DIRECTION('ref_axis',(1.,0.,0.));
#13539=DIRECTION('',(0.,-1.,0.));
#13540=DIRECTION('center_axis',(0.,1.,0.));
#13541=DIRECTION('ref_axis',(0.987688340595138,0.,-0.156434465040232));
#13542=DIRECTION('',(0.,1.,0.));
#13543=DIRECTION('center_axis',(0.,1.,0.));
#13544=DIRECTION('ref_axis',(1.,0.,0.));
#13545=DIRECTION('',(0.,-1.,0.));
#13546=DIRECTION('center_axis',(0.,1.,0.));
#13547=DIRECTION('ref_axis',(1.,0.,2.44929359829471E-16));
#13548=DIRECTION('',(0.,1.,0.));
#13549=DIRECTION('center_axis',(0.,1.,0.));
#13550=DIRECTION('ref_axis',(1.,0.,0.));
#13551=DIRECTION('',(0.,-1.,0.));
#13552=DIRECTION('center_axis',(0.,1.,0.));
#13553=DIRECTION('ref_axis',(0.987688340595137,0.,0.156434465040232));
#13554=DIRECTION('',(0.,1.,0.));
#13555=DIRECTION('center_axis',(0.,1.,0.));
#13556=DIRECTION('ref_axis',(1.,0.,0.));
#13557=DIRECTION('',(0.,-1.,0.));
#13558=DIRECTION('center_axis',(0.,1.,0.));
#13559=DIRECTION('ref_axis',(0.951056516295154,0.,0.309016994374946));
#13560=DIRECTION('',(0.,1.,0.));
#13561=DIRECTION('center_axis',(0.,1.,0.));
#13562=DIRECTION('ref_axis',(1.,0.,0.));
#13563=DIRECTION('',(0.,-1.,0.));
#13564=DIRECTION('center_axis',(0.,1.,0.));
#13565=DIRECTION('ref_axis',(0.891006524188368,0.,0.453990499739547));
#13566=DIRECTION('',(0.,1.,0.));
#13567=DIRECTION('center_axis',(0.,1.,0.));
#13568=DIRECTION('ref_axis',(1.,0.,0.));
#13569=DIRECTION('',(0.,-1.,0.));
#13570=DIRECTION('center_axis',(0.,1.,0.));
#13571=DIRECTION('ref_axis',(0.809016994374947,0.,0.587785252292473));
#13572=DIRECTION('',(0.,1.,0.));
#13573=DIRECTION('center_axis',(0.,1.,0.));
#13574=DIRECTION('ref_axis',(1.,0.,0.));
#13575=DIRECTION('',(0.,-1.,0.));
#13576=DIRECTION('center_axis',(0.,1.,0.));
#13577=DIRECTION('ref_axis',(0.707106781186547,0.,0.707106781186548));
#13578=DIRECTION('',(0.,1.,0.));
#13579=DIRECTION('center_axis',(0.,1.,0.));
#13580=DIRECTION('ref_axis',(1.,0.,0.));
#13581=DIRECTION('',(0.,-1.,0.));
#13582=DIRECTION('center_axis',(0.,1.,0.));
#13583=DIRECTION('ref_axis',(0.587785252292475,0.,0.809016994374946));
#13584=DIRECTION('',(0.,1.,0.));
#13585=DIRECTION('center_axis',(0.,1.,0.));
#13586=DIRECTION('ref_axis',(1.,0.,0.));
#13587=DIRECTION('',(0.,-1.,0.));
#13588=DIRECTION('center_axis',(0.,1.,0.));
#13589=DIRECTION('ref_axis',(0.453990499739547,0.,0.891006524188368));
#13590=DIRECTION('',(0.,1.,0.));
#13591=DIRECTION('center_axis',(0.,1.,0.));
#13592=DIRECTION('ref_axis',(1.,0.,0.));
#13593=DIRECTION('',(0.,-1.,0.));
#13594=DIRECTION('center_axis',(0.,1.,0.));
#13595=DIRECTION('ref_axis',(0.309016994374946,0.,0.951056516295154));
#13596=DIRECTION('',(0.,1.,0.));
#13597=DIRECTION('center_axis',(0.,1.,0.));
#13598=DIRECTION('ref_axis',(1.,0.,0.));
#13599=DIRECTION('',(0.,-1.,0.));
#13600=DIRECTION('center_axis',(0.,1.,0.));
#13601=DIRECTION('ref_axis',(0.156434465040232,0.,0.987688340595138));
#13602=DIRECTION('',(0.,1.,0.));
#13603=DIRECTION('center_axis',(0.,1.,0.));
#13604=DIRECTION('ref_axis',(1.,0.,0.));
#13605=DIRECTION('',(0.,-1.,0.));
#13606=DIRECTION('center_axis',(0.,1.,0.));
#13607=DIRECTION('ref_axis',(-1.83697019872103E-16,0.,1.));
#13608=DIRECTION('',(0.,1.,0.));
#13609=DIRECTION('center_axis',(0.,1.,0.));
#13610=DIRECTION('ref_axis',(1.,0.,0.));
#13611=DIRECTION('',(0.,-1.,0.));
#13612=DIRECTION('center_axis',(0.,1.,0.));
#13613=DIRECTION('ref_axis',(-0.156434465040232,0.,0.987688340595138));
#13614=DIRECTION('',(0.,1.,0.));
#13615=DIRECTION('center_axis',(0.,1.,0.));
#13616=DIRECTION('ref_axis',(1.,0.,0.));
#13617=DIRECTION('',(0.,-1.,0.));
#13618=DIRECTION('center_axis',(0.,1.,0.));
#13619=DIRECTION('ref_axis',(-0.309016994374946,0.,0.951056516295154));
#13620=DIRECTION('',(0.,1.,0.));
#13621=DIRECTION('center_axis',(0.,1.,0.));
#13622=DIRECTION('ref_axis',(1.,0.,0.));
#13623=DIRECTION('',(0.,-1.,0.));
#13624=DIRECTION('center_axis',(0.,1.,0.));
#13625=DIRECTION('ref_axis',(-0.453990499739549,0.,0.891006524188367));
#13626=DIRECTION('',(0.,1.,0.));
#13627=DIRECTION('center_axis',(0.,1.,0.));
#13628=DIRECTION('ref_axis',(1.,0.,0.));
#13629=DIRECTION('',(0.,-1.,0.));
#13630=DIRECTION('center_axis',(0.,1.,0.));
#13631=DIRECTION('ref_axis',(-0.587785252292474,0.,0.809016994374947));
#13632=DIRECTION('',(0.,1.,0.));
#13633=DIRECTION('center_axis',(0.,1.,0.));
#13634=DIRECTION('ref_axis',(1.,0.,0.));
#13635=DIRECTION('',(0.,-1.,0.));
#13636=DIRECTION('center_axis',(0.,1.,0.));
#13637=DIRECTION('ref_axis',(-0.707106781186548,0.,0.707106781186547));
#13638=DIRECTION('',(0.,1.,0.));
#13639=DIRECTION('center_axis',(0.,1.,0.));
#13640=DIRECTION('ref_axis',(1.,0.,0.));
#13641=DIRECTION('',(0.,-1.,0.));
#13642=DIRECTION('center_axis',(0.,1.,0.));
#13643=DIRECTION('ref_axis',(-0.809016994374947,0.,0.587785252292474));
#13644=DIRECTION('',(0.,1.,0.));
#13645=DIRECTION('center_axis',(0.,1.,0.));
#13646=DIRECTION('ref_axis',(1.,0.,0.));
#13647=DIRECTION('',(0.,-1.,0.));
#13648=DIRECTION('center_axis',(0.,1.,0.));
#13649=DIRECTION('ref_axis',(-0.891006524188368,0.,0.453990499739547));
#13650=DIRECTION('',(0.,1.,0.));
#13651=DIRECTION('center_axis',(0.,1.,0.));
#13652=DIRECTION('ref_axis',(1.,0.,0.));
#13653=DIRECTION('',(0.,-1.,0.));
#13654=DIRECTION('center_axis',(0.,1.,0.));
#13655=DIRECTION('ref_axis',(-0.951056516295154,0.,0.309016994374948));
#13656=DIRECTION('',(0.,1.,0.));
#13657=DIRECTION('center_axis',(0.,1.,0.));
#13658=DIRECTION('ref_axis',(1.,0.,0.));
#13659=DIRECTION('',(0.,-1.,0.));
#13660=DIRECTION('center_axis',(0.,1.,0.));
#13661=DIRECTION('ref_axis',(-0.987688340595137,0.,0.156434465040233));
#13662=DIRECTION('',(0.,1.,0.));
#13663=DIRECTION('center_axis',(0.,1.,0.));
#13664=DIRECTION('ref_axis',(1.,0.,0.));
#13665=DIRECTION('',(0.,1.,0.));
#13666=DIRECTION('center_axis',(0.,1.,0.));
#13667=DIRECTION('ref_axis',(-1.,0.,-1.22464679914735E-16));
#13668=DIRECTION('',(0.,-1.,0.));
#13669=DIRECTION('center_axis',(0.,1.,0.));
#13670=DIRECTION('ref_axis',(1.,0.,0.));
#13671=DIRECTION('axis',(0.,0.,1.));
#13672=DIRECTION('refdir',(1.,0.,0.));
#13673=DIRECTION('center_axis',(0.,1.,0.));
#13674=DIRECTION('ref_axis',(0.,0.,1.));
#13675=DIRECTION('center_axis',(0.,-1.,0.));
#13676=DIRECTION('ref_axis',(1.,0.,0.));
#13677=DIRECTION('center_axis',(0.,-1.,0.));
#13678=DIRECTION('ref_axis',(1.,0.,0.));
#13679=DIRECTION('center_axis',(0.,-1.,0.));
#13680=DIRECTION('ref_axis',(1.,0.,0.));
#13681=DIRECTION('',(0.707106781186547,0.707106781186548,8.65956056235493E-17));
#13682=DIRECTION('center_axis',(0.,-1.,0.));
#13683=DIRECTION('ref_axis',(1.,0.,0.));
#13684=DIRECTION('center_axis',(0.,-1.,0.));
#13685=DIRECTION('ref_axis',(1.,0.,0.));
#13686=DIRECTION('',(0.,1.,0.));
#13687=DIRECTION('center_axis',(0.,1.,0.));
#13688=DIRECTION('ref_axis',(1.,0.,0.));
#13689=DIRECTION('center_axis',(0.,-1.,0.));
#13690=DIRECTION('ref_axis',(1.,0.,0.));
#13691=DIRECTION('',(-0.707106781186547,0.707106781186548,-8.65956056235493E-17));
#13692=DIRECTION('center_axis',(0.,-1.,0.));
#13693=DIRECTION('ref_axis',(0.,0.,-1.));
#13694=DIRECTION('center_axis',(0.,-1.,0.));
#13695=DIRECTION('ref_axis',(1.,0.,0.));
#13696=DIRECTION('center_axis',(0.,1.,0.));
#13697=DIRECTION('ref_axis',(1.,0.,0.));
#13698=DIRECTION('center_axis',(0.,1.,0.));
#13699=DIRECTION('ref_axis',(1.,0.,0.));
#13700=DIRECTION('',(-0.447213595499958,0.894427190999916,-5.47678698264203E-17));
#13701=DIRECTION('center_axis',(0.,-1.,0.));
#13702=DIRECTION('ref_axis',(1.,0.,0.));
#13703=DIRECTION('center_axis',(0.,1.,0.));
#13704=DIRECTION('ref_axis',(1.,0.,0.));
#13705=DIRECTION('',(0.,1.,0.));
#13706=DIRECTION('center_axis',(0.,1.,0.));
#13707=DIRECTION('ref_axis',(1.,0.,0.));
#13708=DIRECTION('center_axis',(0.,-1.,0.));
#13709=DIRECTION('ref_axis',(1.,0.,0.));
#13710=DIRECTION('',(-0.707106781186547,0.707106781186548,-8.65956056235493E-17));
#13711=DIRECTION('center_axis',(0.,-1.,0.));
#13712=DIRECTION('ref_axis',(0.,0.,-1.));
#13713=DIRECTION('center_axis',(0.866025403784439,0.,-0.5));
#13714=DIRECTION('ref_axis',(0.5,0.,0.866025403784439));
#13715=DIRECTION('',(-0.5,0.,-0.866025403784439));
#13716=DIRECTION('',(0.,-1.,0.));
#13717=DIRECTION('',(0.5,0.,0.866025403784439));
#13718=DIRECTION('',(0.,-1.,0.));
#13719=DIRECTION('center_axis',(1.60246890531964E-16,0.,-1.));
#13720=DIRECTION('ref_axis',(1.,0.,1.60246890531964E-16));
#13721=DIRECTION('',(-1.,0.,-1.60246890531964E-16));
#13722=DIRECTION('',(0.,-1.,0.));
#13723=DIRECTION('',(1.,0.,1.60246890531964E-16));
#13724=DIRECTION('center_axis',(-0.866025403784439,0.,-0.5));
#13725=DIRECTION('ref_axis',(0.5,0.,-0.866025403784439));
#13726=DIRECTION('',(-0.5,0.,0.866025403784439));
#13727=DIRECTION('',(0.,-1.,0.));
#13728=DIRECTION('',(0.5,0.,-0.866025403784439));
#13729=DIRECTION('center_axis',(-0.866025403784439,0.,0.5));
#13730=DIRECTION('ref_axis',(-0.5,0.,-0.866025403784439));
#13731=DIRECTION('',(0.5,0.,0.866025403784439));
#13732=DIRECTION('',(0.,-1.,0.));
#13733=DIRECTION('',(-0.5,0.,-0.866025403784439));
#13734=DIRECTION('center_axis',(-1.60246890531964E-16,0.,1.));
#13735=DIRECTION('ref_axis',(-1.,0.,-1.60246890531964E-16));
#13736=DIRECTION('',(1.,0.,1.60246890531964E-16));
#13737=DIRECTION('',(0.,-1.,0.));
#13738=DIRECTION('',(-1.,0.,-1.60246890531964E-16));
#13739=DIRECTION('center_axis',(0.866025403784439,0.,0.5));
#13740=DIRECTION('ref_axis',(-0.5,0.,0.866025403784439));
#13741=DIRECTION('',(0.5,0.,-0.866025403784439));
#13742=DIRECTION('',(-0.5,0.,0.866025403784439));
#13743=DIRECTION('center_axis',(0.,1.,0.));
#13744=DIRECTION('ref_axis',(1.,0.,0.));
#13745=DIRECTION('center_axis',(0.,-1.,0.));
#13746=DIRECTION('ref_axis',(0.,0.,-1.));
#13747=DIRECTION('',(0.,0.,1.));
#13748=DIRECTION('',(1.,0.,0.));
#13749=DIRECTION('',(0.,0.,1.));
#13750=DIRECTION('',(1.,0.,0.));
#13751=DIRECTION('',(0.,0.,1.));
#13752=DIRECTION('',(1.,0.,0.));
#13753=DIRECTION('',(0.,0.,1.));
#13754=DIRECTION('',(1.,0.,0.));
#13755=DIRECTION('',(0.,0.,1.));
#13756=DIRECTION('',(1.,0.,0.));
#13757=DIRECTION('',(0.,0.,1.));
#13758=DIRECTION('',(1.,0.,0.));
#13759=DIRECTION('',(0.,0.,1.));
#13760=DIRECTION('',(1.,0.,0.));
#13761=DIRECTION('',(0.,0.,1.));
#13762=DIRECTION('',(1.,0.,0.));
#13763=DIRECTION('',(0.,0.,1.));
#13764=DIRECTION('',(1.,0.,0.));
#13765=DIRECTION('',(0.,0.,1.));
#13766=DIRECTION('',(1.,0.,0.));
#13767=DIRECTION('',(0.,0.,1.));
#13768=DIRECTION('',(1.,0.,0.));
#13769=DIRECTION('',(0.,0.,1.));
#13770=DIRECTION('',(1.,0.,0.));
#13771=DIRECTION('',(0.,0.,1.));
#13772=DIRECTION('',(1.,0.,0.));
#13773=DIRECTION('',(0.,0.,1.));
#13774=DIRECTION('',(1.,0.,0.));
#13775=DIRECTION('',(0.,0.,1.));
#13776=DIRECTION('',(1.,0.,0.));
#13777=DIRECTION('',(0.,0.,1.));
#13778=DIRECTION('',(1.,0.,0.));
#13779=DIRECTION('',(0.,-1.,2.22044604925031E-16));
#13780=DIRECTION('',(1.,0.,0.));
#13781=DIRECTION('',(0.,-1.,2.22044604925031E-16));
#13782=DIRECTION('',(1.,0.,0.));
#13783=DIRECTION('',(0.,-1.,2.22044604925031E-16));
#13784=DIRECTION('',(1.,0.,0.));
#13785=DIRECTION('',(0.,-1.,2.22044604925031E-16));
#13786=DIRECTION('',(1.,0.,0.));
#13787=DIRECTION('',(0.,0.,1.));
#13788=DIRECTION('',(1.,0.,0.));
#13789=DIRECTION('',(0.,0.,1.));
#13790=DIRECTION('',(1.,0.,0.));
#13791=DIRECTION('',(0.,0.,1.));
#13792=DIRECTION('',(-1.,1.22464679914735E-16,0.));
#13793=DIRECTION('',(0.,0.,1.));
#13794=DIRECTION('',(-1.,1.22464679914735E-16,0.));
#13795=DIRECTION('',(0.,0.,1.));
#13796=DIRECTION('',(-1.,1.22464679914735E-16,0.));
#13797=DIRECTION('',(0.,0.,1.));
#13798=DIRECTION('',(-1.,1.22464679914735E-16,0.));
#13799=DIRECTION('',(0.,0.,1.));
#13800=DIRECTION('',(1.,0.,0.));
#13801=DIRECTION('',(0.,0.,1.));
#13802=DIRECTION('',(1.,0.,0.));
#13803=DIRECTION('',(0.,0.,1.));
#13804=DIRECTION('',(1.,0.,0.));
#13805=DIRECTION('',(0.,0.,1.));
#13806=DIRECTION('',(1.,0.,0.));
#13807=DIRECTION('',(0.,-1.,2.22044604925031E-16));
#13808=DIRECTION('',(1.,0.,0.));
#13809=DIRECTION('',(0.,-1.,2.22044604925031E-16));
#13810=DIRECTION('',(1.,0.,0.));
#13811=DIRECTION('',(0.,-1.,2.22044604925031E-16));
#13812=DIRECTION('',(1.,0.,0.));
#13813=DIRECTION('',(0.,-1.,2.22044604925031E-16));
#13814=DIRECTION('',(1.,0.,0.));
#13815=DIRECTION('',(0.,0.,1.));
#13816=DIRECTION('',(1.,0.,0.));
#13817=DIRECTION('',(0.,0.,1.));
#13818=DIRECTION('',(1.,0.,0.));
#13819=DIRECTION('',(0.,0.,1.));
#13820=DIRECTION('',(-1.,1.22464679914735E-16,0.));
#13821=DIRECTION('',(0.,0.,1.));
#13822=DIRECTION('',(-1.,1.22464679914735E-16,0.));
#13823=DIRECTION('',(0.,0.,1.));
#13824=DIRECTION('',(-1.,1.22464679914735E-16,0.));
#13825=DIRECTION('',(0.,0.,1.));
#13826=DIRECTION('',(-1.,1.22464679914735E-16,0.));
#13827=DIRECTION('',(0.,0.,1.));
#13828=DIRECTION('',(1.,0.,0.));
#13829=DIRECTION('',(0.,0.,1.));
#13830=DIRECTION('',(1.,0.,0.));
#13831=DIRECTION('',(0.,0.,1.));
#13832=DIRECTION('',(1.,0.,0.));
#13833=DIRECTION('',(0.,0.,1.));
#13834=DIRECTION('',(1.,0.,0.));
#13835=DIRECTION('',(0.,0.,1.));
#13836=DIRECTION('',(1.,0.,0.));
#13837=DIRECTION('',(0.,0.,1.));
#13838=DIRECTION('',(1.,0.,0.));
#13839=DIRECTION('',(0.,0.,1.));
#13840=DIRECTION('',(1.,0.,0.));
#13841=DIRECTION('',(0.,0.,1.));
#13842=DIRECTION('',(1.,0.,0.));
#13843=DIRECTION('',(0.,0.,1.));
#13844=DIRECTION('',(1.,0.,0.));
#13845=DIRECTION('',(0.,0.,1.));
#13846=DIRECTION('',(1.,0.,0.));
#13847=DIRECTION('',(0.,0.,1.));
#13848=DIRECTION('',(1.,0.,0.));
#13849=DIRECTION('',(0.,0.,1.));
#13850=DIRECTION('',(-1.,1.22464679914735E-16,0.));
#13851=DIRECTION('',(0.,0.,1.));
#13852=DIRECTION('',(1.,0.,0.));
#13853=DIRECTION('',(0.,0.,1.));
#13854=DIRECTION('',(1.,0.,0.));
#13855=DIRECTION('',(0.,0.,1.));
#13856=DIRECTION('',(1.,0.,0.));
#13857=DIRECTION('',(0.,0.,1.));
#13858=DIRECTION('',(1.,0.,0.));
#13859=DIRECTION('',(0.,0.,1.));
#13860=DIRECTION('',(1.,0.,0.));
#13861=DIRECTION('',(0.,0.,1.));
#13862=DIRECTION('',(1.,0.,0.));
#13863=DIRECTION('',(0.,0.,1.));
#13864=DIRECTION('',(1.,0.,0.));
#13865=DIRECTION('',(0.,0.,1.));
#13866=DIRECTION('',(-1.,1.22464679914735E-16,0.));
#13867=DIRECTION('',(0.,0.,1.));
#13868=DIRECTION('',(1.,0.,0.));
#13869=DIRECTION('',(0.,0.,1.));
#13870=DIRECTION('',(1.,0.,0.));
#13871=DIRECTION('',(0.,0.,1.));
#13872=DIRECTION('',(1.,0.,0.));
#13873=CARTESIAN_POINT('',(0.,0.,0.));
#13874=CARTESIAN_POINT('',(0.,0.,0.));
#13875=CARTESIAN_POINT('',(0.,0.,0.));
#13876=CARTESIAN_POINT('Origin',(8.77091003018116,1.,-1.3));
#13877=CARTESIAN_POINT('',(8.77091003018116,0.775,-1.2));
#13878=CARTESIAN_POINT('',(8.77091003018116,0.775,0.));
#13879=CARTESIAN_POINT('',(8.77091003018116,0.775,-1.3));
#13880=CARTESIAN_POINT('',(8.77091003018116,1.225,-1.2));
#13881=CARTESIAN_POINT('Origin',(8.77091003018116,1.,-1.2));
#13882=CARTESIAN_POINT('',(8.77091003018116,1.225,0.));
#13883=CARTESIAN_POINT('',(8.77091003018116,1.225,-1.3));
#13884=CARTESIAN_POINT('Origin',(8.77091003018116,1.,0.));
#13885=CARTESIAN_POINT('Origin',(10.7709100301812,1.,-1.3));
#13886=CARTESIAN_POINT('',(10.7709100301812,0.775,-1.2));
#13887=CARTESIAN_POINT('',(10.7709100301812,0.775,0.));
#13888=CARTESIAN_POINT('',(10.7709100301812,0.775,-1.3));
#13889=CARTESIAN_POINT('',(10.7709100301812,1.225,0.));
#13890=CARTESIAN_POINT('Origin',(10.7709100301812,1.,0.));
#13891=CARTESIAN_POINT('',(10.7709100301812,1.225,-1.2));
#13892=CARTESIAN_POINT('',(10.7709100301812,1.225,-1.3));
#13893=CARTESIAN_POINT('Origin',(10.7709100301812,1.,-1.2));
#13894=CARTESIAN_POINT('Origin',(4.,-1.,-1.2));
#13895=CARTESIAN_POINT('',(-4.,4.5,-1.2));
#13896=CARTESIAN_POINT('',(-4.,-6.5,-1.2));
#13897=CARTESIAN_POINT('',(-4.,4.5,-1.2));
#13898=CARTESIAN_POINT('',(12.,4.5,-1.2));
#13899=CARTESIAN_POINT('',(12.,4.5,-1.2));
#13900=CARTESIAN_POINT('',(12.,-6.5,-1.2));
#13901=CARTESIAN_POINT('',(12.,-6.5,-1.2));
#13902=CARTESIAN_POINT('',(-4.,-6.5,-1.2));
#13903=CARTESIAN_POINT('',(8.77091003018116,-0.775,-1.2));
#13904=CARTESIAN_POINT('',(8.77091003018116,-1.225,-1.2));
#13905=CARTESIAN_POINT('Origin',(8.77091003018116,-1.,-1.2));
#13906=CARTESIAN_POINT('',(10.7709100301812,-1.225,-1.2));
#13907=CARTESIAN_POINT('',(6.38545501509058,-1.225,-1.2));
#13908=CARTESIAN_POINT('',(10.7709100301812,-0.775,-1.2));
#13909=CARTESIAN_POINT('Origin',(10.7709100301812,-1.,-1.2));
#13910=CARTESIAN_POINT('',(7.38545501509058,-0.775,-1.2));
#13911=CARTESIAN_POINT('',(3.17091003018116,-0.775,-1.2));
#13912=CARTESIAN_POINT('',(3.17091003018116,-1.225,-1.2));
#13913=CARTESIAN_POINT('Origin',(3.17091003018116,-1.,-1.2));
#13914=CARTESIAN_POINT('',(5.17091003018116,-1.225,-1.2));
#13915=CARTESIAN_POINT('',(3.58545501509058,-1.225,-1.2));
#13916=CARTESIAN_POINT('',(5.17091003018116,-0.775,-1.2));
#13917=CARTESIAN_POINT('Origin',(5.17091003018116,-1.,-1.2));
#13918=CARTESIAN_POINT('',(4.58545501509058,-0.775,-1.2));
#13919=CARTESIAN_POINT('',(3.17091003018116,1.225,-1.2));
#13920=CARTESIAN_POINT('',(3.17091003018116,0.775,-1.2));
#13921=CARTESIAN_POINT('Origin',(3.17091003018116,1.,-1.2));
#13922=CARTESIAN_POINT('',(5.17091003018116,0.775,-1.2));
#13923=CARTESIAN_POINT('',(3.58545501509058,0.775,-1.2));
#13924=CARTESIAN_POINT('',(5.17091003018116,1.225,-1.2));
#13925=CARTESIAN_POINT('Origin',(5.17091003018116,1.,-1.2));
#13926=CARTESIAN_POINT('',(4.58545501509058,1.225,-1.2));
#13927=CARTESIAN_POINT('',(6.38545501509058,0.775,-1.2));
#13928=CARTESIAN_POINT('',(7.38545501509058,1.225,-1.2));
#13929=CARTESIAN_POINT('Origin',(10.7709100301812,1.225,-1.3));
#13930=CARTESIAN_POINT('',(7.38545501509058,1.225,0.));
#13931=CARTESIAN_POINT('Origin',(8.77091003018116,0.775,-1.3));
#13932=CARTESIAN_POINT('',(6.38545501509058,0.775,0.));
#13933=CARTESIAN_POINT('Origin',(8.77091003018116,-1.,-1.3));
#13934=CARTESIAN_POINT('',(8.77091003018116,-1.225,0.));
#13935=CARTESIAN_POINT('',(8.77091003018116,-1.225,-1.3));
#13936=CARTESIAN_POINT('',(8.77091003018116,-0.775,0.));
#13937=CARTESIAN_POINT('',(8.77091003018116,-0.775,-1.3));
#13938=CARTESIAN_POINT('Origin',(8.77091003018116,-1.,0.));
#13939=CARTESIAN_POINT('Origin',(10.7709100301812,-1.,-1.3));
#13940=CARTESIAN_POINT('',(10.7709100301812,-1.225,0.));
#13941=CARTESIAN_POINT('',(10.7709100301812,-1.225,-1.3));
#13942=CARTESIAN_POINT('',(10.7709100301812,-0.775,0.));
#13943=CARTESIAN_POINT('Origin',(10.7709100301812,-1.,0.));
#13944=CARTESIAN_POINT('',(10.7709100301812,-0.775,-1.3));
#13945=CARTESIAN_POINT('Origin',(10.7709100301812,-0.775,-1.3));
#13946=CARTESIAN_POINT('',(7.38545501509058,-0.775,0.));
#13947=CARTESIAN_POINT('Origin',(8.77091003018116,-1.225,-1.3));
#13948=CARTESIAN_POINT('',(6.38545501509058,-1.225,0.));
#13949=CARTESIAN_POINT('Origin',(3.17091003018116,1.,-1.3));
#13950=CARTESIAN_POINT('',(2.9539109773241,0.940532268757414,0.));
#13951=CARTESIAN_POINT('',(2.9539109773241,0.940532268757414,-1.1));
#13952=CARTESIAN_POINT('',(2.9539109773241,0.940532268757414,-1.3));
#13953=CARTESIAN_POINT('',(3.17091003018116,0.775,0.));
#13954=CARTESIAN_POINT('Origin',(3.17091003018116,1.,0.));
#13955=CARTESIAN_POINT('',(3.17091003018116,0.775,-1.3));
#13956=CARTESIAN_POINT('',(3.17091003018116,1.225,0.));
#13957=CARTESIAN_POINT('',(3.17091003018116,1.225,-1.3));
#13958=CARTESIAN_POINT('',(2.9539109773241,1.05946773124259,0.));
#13959=CARTESIAN_POINT('Origin',(3.17091003018116,1.,0.));
#13960=CARTESIAN_POINT('',(2.9539109773241,1.05946773124259,-1.1));
#13961=CARTESIAN_POINT('',(2.9539109773241,1.05946773124259,-1.3));
#13962=CARTESIAN_POINT('Origin',(3.17091003018116,1.,-1.1));
#13963=CARTESIAN_POINT('Origin',(5.17091003018116,1.,-1.3));
#13964=CARTESIAN_POINT('',(5.17091003018116,0.775,0.));
#13965=CARTESIAN_POINT('',(5.17091003018116,0.775,-1.3));
#13966=CARTESIAN_POINT('',(5.17091003018116,1.225,0.));
#13967=CARTESIAN_POINT('Origin',(5.17091003018116,1.,0.));
#13968=CARTESIAN_POINT('',(5.17091003018116,1.225,-1.3));
#13969=CARTESIAN_POINT('Origin',(5.17091003018116,1.225,-1.3));
#13970=CARTESIAN_POINT('',(4.58545501509058,1.225,0.));
#13971=CARTESIAN_POINT('Origin',(3.17091003018116,0.775,-1.3));
#13972=CARTESIAN_POINT('',(3.58545501509058,0.775,0.));
#13973=CARTESIAN_POINT('Origin',(3.17091003018116,-1.,-1.3));
#13974=CARTESIAN_POINT('',(2.9539109773241,-1.05946773124259,0.));
#13975=CARTESIAN_POINT('',(2.9539109773241,-1.05946773124259,-1.1));
#13976=CARTESIAN_POINT('',(2.9539109773241,-1.05946773124259,-1.3));
#13977=CARTESIAN_POINT('',(3.17091003018116,-1.225,0.));
#13978=CARTESIAN_POINT('Origin',(3.17091003018116,-1.,0.));
#13979=CARTESIAN_POINT('',(3.17091003018116,-1.225,-1.3));
#13980=CARTESIAN_POINT('',(3.17091003018116,-0.775,0.));
#13981=CARTESIAN_POINT('',(3.17091003018116,-0.775,-1.3));
#13982=CARTESIAN_POINT('',(2.9539109773241,-0.940532268757414,0.));
#13983=CARTESIAN_POINT('Origin',(3.17091003018116,-1.,0.));
#13984=CARTESIAN_POINT('',(2.9539109773241,-0.940532268757414,-1.1));
#13985=CARTESIAN_POINT('',(2.9539109773241,-0.940532268757414,-1.3));
#13986=CARTESIAN_POINT('Origin',(3.17091003018116,-1.,-1.1));
#13987=CARTESIAN_POINT('Origin',(5.17091003018116,-1.,-1.3));
#13988=CARTESIAN_POINT('',(5.17091003018116,-1.225,0.));
#13989=CARTESIAN_POINT('',(5.17091003018116,-1.225,-1.3));
#13990=CARTESIAN_POINT('',(5.17091003018116,-0.775,0.));
#13991=CARTESIAN_POINT('Origin',(5.17091003018116,-1.,0.));
#13992=CARTESIAN_POINT('',(5.17091003018116,-0.775,-1.3));
#13993=CARTESIAN_POINT('Origin',(5.17091003018116,-0.775,-1.3));
#13994=CARTESIAN_POINT('',(4.58545501509058,-0.775,0.));
#13995=CARTESIAN_POINT('Origin',(3.17091003018116,-1.225,-1.3));
#13996=CARTESIAN_POINT('',(3.58545501509058,-1.225,0.));
#13997=CARTESIAN_POINT('Origin',(2.8,-1.,-1.1));
#13998=CARTESIAN_POINT('Origin',(2.8,-1.,0.));
#13999=CARTESIAN_POINT('Origin',(2.8,-1.,-1.1));
#14000=CARTESIAN_POINT('Origin',(2.8,-1.,-1.1));
#14001=CARTESIAN_POINT('Origin',(-2.8,1.,-1.1));
#14002=CARTESIAN_POINT('',(-2.965,1.,-1.1));
#14003=CARTESIAN_POINT('Origin',(-2.8,1.,-1.1));
#14004=CARTESIAN_POINT('',(-2.965,1.,0.));
#14005=CARTESIAN_POINT('',(-2.965,1.,-1.1));
#14006=CARTESIAN_POINT('Origin',(-2.8,1.,0.));
#14007=CARTESIAN_POINT('Origin',(-2.8,1.,-1.1));
#14008=CARTESIAN_POINT('Origin',(-2.8,-1.,-1.1));
#14009=CARTESIAN_POINT('',(-2.965,-1.,-1.1));
#14010=CARTESIAN_POINT('Origin',(-2.8,-1.,-1.1));
#14011=CARTESIAN_POINT('',(-2.965,-1.,0.));
#14012=CARTESIAN_POINT('',(-2.965,-1.,-1.1));
#14013=CARTESIAN_POINT('Origin',(-2.8,-1.,0.));
#14014=CARTESIAN_POINT('Origin',(-2.8,-1.,-1.1));
#14015=CARTESIAN_POINT('Origin',(2.8,1.,-1.1));
#14016=CARTESIAN_POINT('Origin',(2.8,1.,0.));
#14017=CARTESIAN_POINT('Origin',(2.8,1.,-1.1));
#14018=CARTESIAN_POINT('Origin',(2.8,1.,-1.1));
#14019=CARTESIAN_POINT('Origin',(12.,4.5,-1.2));
#14020=CARTESIAN_POINT('',(-4.,4.5,0.));
#14021=CARTESIAN_POINT('',(-4.,4.5,-1.2));
#14022=CARTESIAN_POINT('',(12.,4.5,0.));
#14023=CARTESIAN_POINT('',(12.,4.5,0.));
#14024=CARTESIAN_POINT('',(12.,4.5,-1.2));
#14025=CARTESIAN_POINT('Origin',(12.,-6.5,-1.2));
#14026=CARTESIAN_POINT('',(12.,-6.5,0.));
#14027=CARTESIAN_POINT('',(12.,-6.5,0.));
#14028=CARTESIAN_POINT('',(12.,-6.5,-1.2));
#14029=CARTESIAN_POINT('Origin',(-4.,-6.5,-1.2));
#14030=CARTESIAN_POINT('',(-4.,-6.5,0.));
#14031=CARTESIAN_POINT('',(-4.,-6.5,0.));
#14032=CARTESIAN_POINT('',(-4.,-6.5,-1.2));
#14033=CARTESIAN_POINT('Origin',(-4.,4.5,-1.2));
#14034=CARTESIAN_POINT('',(-4.,4.5,0.));
#14035=CARTESIAN_POINT('Origin',(4.,-1.,0.));
#14036=CARTESIAN_POINT('',(0.,0.,0.));
#14037=CARTESIAN_POINT('Origin',(-3.,4.5,-2.4));
#14038=CARTESIAN_POINT('',(-3.,4.5,-2.4));
#14039=CARTESIAN_POINT('',(-4.,4.5,-2.4));
#14040=CARTESIAN_POINT('',(-3.,4.5,-2.4));
#14041=CARTESIAN_POINT('',(-4.,4.5,-1.2));
#14042=CARTESIAN_POINT('',(-4.,4.5,-2.4));
#14043=CARTESIAN_POINT('',(-3.,4.5,-1.2));
#14044=CARTESIAN_POINT('',(-3.,4.5,-1.2));
#14045=CARTESIAN_POINT('',(-3.,4.5,-2.4));
#14046=CARTESIAN_POINT('Origin',(-3.,-6.5,-2.4));
#14047=CARTESIAN_POINT('',(-3.,-6.5,-2.4));
#14048=CARTESIAN_POINT('',(-3.,-6.5,-2.4));
#14049=CARTESIAN_POINT('',(-3.,-6.5,-1.2));
#14050=CARTESIAN_POINT('',(-3.,-6.5,-1.2));
#14051=CARTESIAN_POINT('',(-3.,-6.5,-2.4));
#14052=CARTESIAN_POINT('Origin',(-4.,-6.5,-2.4));
#14053=CARTESIAN_POINT('',(-4.,-6.5,-2.4));
#14054=CARTESIAN_POINT('',(-4.,-6.5,-2.4));
#14055=CARTESIAN_POINT('',(-4.,-6.5,-1.2));
#14056=CARTESIAN_POINT('',(-4.,-6.5,-1.2));
#14057=CARTESIAN_POINT('',(-4.,-6.5,-2.4));
#14058=CARTESIAN_POINT('Origin',(-4.,4.5,-2.4));
#14059=CARTESIAN_POINT('',(-4.,4.5,-2.4));
#14060=CARTESIAN_POINT('',(-4.,4.5,-1.2));
#14061=CARTESIAN_POINT('Origin',(-3.5,-1.,-1.2));
#14062=CARTESIAN_POINT('Origin',(-3.5,-1.,-2.4));
#14063=CARTESIAN_POINT('',(0.,0.,0.));
#14064=CARTESIAN_POINT('Origin',(12.,4.5,-2.4));
#14065=CARTESIAN_POINT('',(12.,4.5,-2.4));
#14066=CARTESIAN_POINT('',(11.,4.5,-2.4));
#14067=CARTESIAN_POINT('',(12.,4.5,-2.4));
#14068=CARTESIAN_POINT('',(11.,4.5,-1.2));
#14069=CARTESIAN_POINT('',(11.,4.5,-2.4));
#14070=CARTESIAN_POINT('',(12.,4.5,-1.2));
#14071=CARTESIAN_POINT('',(12.,4.5,-1.2));
#14072=CARTESIAN_POINT('',(12.,4.5,-2.4));
#14073=CARTESIAN_POINT('Origin',(12.,-6.5,-2.4));
#14074=CARTESIAN_POINT('',(12.,-6.5,-2.4));
#14075=CARTESIAN_POINT('',(12.,-6.5,-2.4));
#14076=CARTESIAN_POINT('',(12.,-6.5,-1.2));
#14077=CARTESIAN_POINT('',(12.,-6.5,-1.2));
#14078=CARTESIAN_POINT('',(12.,-6.5,-2.4));
#14079=CARTESIAN_POINT('Origin',(11.,-6.5,-2.4));
#14080=CARTESIAN_POINT('',(11.,-6.5,-2.4));
#14081=CARTESIAN_POINT('',(11.,-6.5,-2.4));
#14082=CARTESIAN_POINT('',(11.,-6.5,-1.2));
#14083=CARTESIAN_POINT('',(11.,-6.5,-1.2));
#14084=CARTESIAN_POINT('',(11.,-6.5,-2.4));
#14085=CARTESIAN_POINT('Origin',(11.,4.5,-2.4));
#14086=CARTESIAN_POINT('',(11.,4.5,-2.4));
#14087=CARTESIAN_POINT('',(11.,4.5,-1.2));
#14088=CARTESIAN_POINT('Origin',(11.5,-1.,-1.2));
#14089=CARTESIAN_POINT('Origin',(11.5,-1.,-2.4));
#14090=CARTESIAN_POINT('',(0.,0.,0.));
#14091=CARTESIAN_POINT('Origin',(-1.34350288425444,-1.9,5.65649711574556));
#14092=CARTESIAN_POINT('',(-1.50850288425444,-1.8,5.65649711574556));
#14093=CARTESIAN_POINT('Origin',(-1.34350288425444,-1.8,5.65649711574556));
#14094=CARTESIAN_POINT('',(-1.50850288425444,1.8,5.65649711574556));
#14095=CARTESIAN_POINT('',(-1.50850288425444,-1.9,5.65649711574556));
#14096=CARTESIAN_POINT('Origin',(-1.34350288425444,1.8,5.65649711574556));
#14097=CARTESIAN_POINT('Origin',(-1.34350288425444,-1.9,8.34350288425444));
#14098=CARTESIAN_POINT('',(-1.50850288425444,-1.8,8.34350288425444));
#14099=CARTESIAN_POINT('Origin',(-1.34350288425444,-1.8,8.34350288425444));
#14100=CARTESIAN_POINT('',(-1.50850288425444,1.8,8.34350288425444));
#14101=CARTESIAN_POINT('',(-1.50850288425444,-1.9,8.34350288425444));
#14102=CARTESIAN_POINT('Origin',(-1.34350288425444,1.8,8.34350288425444));
#14103=CARTESIAN_POINT('Origin',(1.34350288425444,-1.9,8.34350288425444));
#14104=CARTESIAN_POINT('',(1.17850288425444,-1.8,8.34350288425444));
#14105=CARTESIAN_POINT('Origin',(1.34350288425444,-1.8,8.34350288425444));
#14106=CARTESIAN_POINT('',(1.17850288425444,1.8,8.34350288425444));
#14107=CARTESIAN_POINT('',(1.17850288425444,-1.9,8.34350288425444));
#14108=CARTESIAN_POINT('Origin',(1.34350288425444,1.8,8.34350288425444));
#14109=CARTESIAN_POINT('Origin',(1.34350288425444,-1.9,5.65649711574556));
#14110=CARTESIAN_POINT('',(1.17850288425444,-1.8,5.65649711574556));
#14111=CARTESIAN_POINT('Origin',(1.34350288425444,-1.8,5.65649711574556));
#14112=CARTESIAN_POINT('',(1.17850288425444,1.8,5.65649711574556));
#14113=CARTESIAN_POINT('',(1.17850288425444,-1.9,5.65649711574556));
#14114=CARTESIAN_POINT('Origin',(1.34350288425444,1.8,5.65649711574556));
#14115=CARTESIAN_POINT('Origin',(0.,-1.9,7.));
#14116=CARTESIAN_POINT('',(-1.5,-1.8,7.));
#14117=CARTESIAN_POINT('Origin',(0.,-1.8,7.));
#14118=CARTESIAN_POINT('',(-1.5,1.8,7.));
#14119=CARTESIAN_POINT('',(-1.5,-1.9,7.));
#14120=CARTESIAN_POINT('Origin',(0.,1.8,7.));
#14121=CARTESIAN_POINT('Origin',(2.8,-1.,-0.1));
#14122=CARTESIAN_POINT('',(2.575,-1.,0.));
#14123=CARTESIAN_POINT('Origin',(2.8,-1.,0.));
#14124=CARTESIAN_POINT('',(2.575,-1.,0.8));
#14125=CARTESIAN_POINT('',(2.575,-1.,-0.1));
#14126=CARTESIAN_POINT('Origin',(2.8,-1.,0.8));
#14127=CARTESIAN_POINT('Origin',(-2.8,1.,-0.1));
#14128=CARTESIAN_POINT('',(-3.025,1.,0.));
#14129=CARTESIAN_POINT('Origin',(-2.8,1.,0.));
#14130=CARTESIAN_POINT('',(-3.025,1.,0.8));
#14131=CARTESIAN_POINT('',(-3.025,1.,-0.1));
#14132=CARTESIAN_POINT('Origin',(-2.8,1.,0.8));
#14133=CARTESIAN_POINT('Origin',(-2.8,-1.,-0.1));
#14134=CARTESIAN_POINT('',(-3.025,-1.,0.));
#14135=CARTESIAN_POINT('Origin',(-2.8,-1.,0.));
#14136=CARTESIAN_POINT('',(-3.025,-1.,0.8));
#14137=CARTESIAN_POINT('',(-3.025,-1.,-0.1));
#14138=CARTESIAN_POINT('Origin',(-2.8,-1.,0.8));
#14139=CARTESIAN_POINT('Origin',(2.8,1.,-0.1));
#14140=CARTESIAN_POINT('',(2.575,1.,0.));
#14141=CARTESIAN_POINT('Origin',(2.8,1.,0.));
#14142=CARTESIAN_POINT('',(2.575,1.,0.8));
#14143=CARTESIAN_POINT('',(2.575,1.,-0.1));
#14144=CARTESIAN_POINT('Origin',(2.8,1.,0.8));
#14145=CARTESIAN_POINT('Origin',(-3.4,-1.8,0.8));
#14146=CARTESIAN_POINT('',(2.2,-1.8,0.8));
#14147=CARTESIAN_POINT('',(2.2,1.8,0.8));
#14148=CARTESIAN_POINT('',(2.2,-1.8,0.8));
#14149=CARTESIAN_POINT('',(3.4,-1.8,0.8));
#14150=CARTESIAN_POINT('',(3.4,-1.8,0.8));
#14151=CARTESIAN_POINT('',(3.4,1.8,0.8));
#14152=CARTESIAN_POINT('',(3.4,-1.8,0.8));
#14153=CARTESIAN_POINT('',(3.4,1.8,0.8));
#14154=CARTESIAN_POINT('Origin',(-3.4,-1.8,0.8));
#14155=CARTESIAN_POINT('',(-2.2,1.8,0.8));
#14156=CARTESIAN_POINT('',(-2.2,-1.8,0.8));
#14157=CARTESIAN_POINT('',(-2.2,0.,0.8));
#14158=CARTESIAN_POINT('',(-3.4,1.8,0.8));
#14159=CARTESIAN_POINT('',(3.4,1.8,0.8));
#14160=CARTESIAN_POINT('',(-3.4,-1.8,0.8));
#14161=CARTESIAN_POINT('',(-3.4,-1.8,0.8));
#14162=CARTESIAN_POINT('',(3.4,-1.8,0.8));
#14163=CARTESIAN_POINT('Origin',(-3.4,-1.8,0.));
#14164=CARTESIAN_POINT('',(-3.4,-1.8,0.));
#14165=CARTESIAN_POINT('',(-3.4,-1.8,0.8));
#14166=CARTESIAN_POINT('',(-3.4,1.8,0.));
#14167=CARTESIAN_POINT('',(-3.4,1.8,0.8));
#14168=CARTESIAN_POINT('',(-3.4,-1.8,0.));
#14169=CARTESIAN_POINT('Origin',(3.4,-1.8,0.8));
#14170=CARTESIAN_POINT('',(3.4,-1.8,0.));
#14171=CARTESIAN_POINT('',(3.4,-1.8,0.));
#14172=CARTESIAN_POINT('',(3.4,1.8,0.));
#14173=CARTESIAN_POINT('',(3.4,-1.8,0.));
#14174=CARTESIAN_POINT('',(3.4,1.8,0.));
#14175=CARTESIAN_POINT('Origin',(-2.2,-1.8,0.));
#14176=CARTESIAN_POINT('',(2.2,-1.8,9.2));
#14177=CARTESIAN_POINT('',(2.2,-1.8,0.));
#14178=CARTESIAN_POINT('',(-2.2,-1.8,9.2));
#14179=CARTESIAN_POINT('',(-2.2,-1.8,9.2));
#14180=CARTESIAN_POINT('',(-2.2,-1.8,0.));
#14181=CARTESIAN_POINT('',(-3.4,-1.8,0.));
#14182=CARTESIAN_POINT('Origin',(2.2,-1.8,0.));
#14183=CARTESIAN_POINT('',(2.2,1.8,9.2));
#14184=CARTESIAN_POINT('',(2.2,1.8,0.));
#14185=CARTESIAN_POINT('',(2.2,-1.8,9.2));
#14186=CARTESIAN_POINT('Origin',(2.2,1.8,0.));
#14187=CARTESIAN_POINT('',(-2.2,1.8,9.2));
#14188=CARTESIAN_POINT('',(-2.2,1.8,0.));
#14189=CARTESIAN_POINT('',(2.2,1.8,9.2));
#14190=CARTESIAN_POINT('',(-3.4,1.8,0.));
#14191=CARTESIAN_POINT('Origin',(-2.2,1.8,0.));
#14192=CARTESIAN_POINT('',(-2.2,1.8,9.2));
#14193=CARTESIAN_POINT('Origin',(0.,0.,9.2));
#14194=CARTESIAN_POINT('Origin',(0.,0.,0.));
#14195=CARTESIAN_POINT('',(0.,0.,0.));
#14196=CARTESIAN_POINT('Origin',(0.,-0.45,7.));
#14197=CARTESIAN_POINT('',(-1.1,0.45,7.));
#14198=CARTESIAN_POINT('Origin',(0.,0.45,7.));
#14199=CARTESIAN_POINT('',(-1.1,-0.45,7.));
#14200=CARTESIAN_POINT('',(-1.1,-0.45,7.));
#14201=CARTESIAN_POINT('Origin',(0.,-0.45,7.));
#14202=CARTESIAN_POINT('Origin',(0.,-0.45,7.));
#14203=CARTESIAN_POINT('',(-1.49,0.45,7.));
#14204=CARTESIAN_POINT('Origin',(0.,0.45,7.));
#14205=CARTESIAN_POINT('',(-1.49,-0.45,7.));
#14206=CARTESIAN_POINT('',(-1.49,-0.45,7.));
#14207=CARTESIAN_POINT('Origin',(0.,-0.45,7.));
#14208=CARTESIAN_POINT('Origin',(0.,0.45,7.));
#14209=CARTESIAN_POINT('Origin',(0.,-0.45,7.));
#14210=CARTESIAN_POINT('',(0.,0.,0.));
#14211=CARTESIAN_POINT('Origin',(-1.34350288425444,-2.2,5.65649711574556));
#14212=CARTESIAN_POINT('',(-1.40634555589641,-2.1,5.4404512904656));
#14213=CARTESIAN_POINT('',(-1.40634555589641,-1.8,5.4404512904656));
#14214=CARTESIAN_POINT('',(-1.40634555589641,-2.2,5.4404512904656));
#14215=CARTESIAN_POINT('',(-1.5595487095344,-2.1,5.59365444410359));
#14216=CARTESIAN_POINT('Origin',(-1.34350288425444,-2.1,5.65649711574556));
#14217=CARTESIAN_POINT('',(-1.5595487095344,-1.8,5.59365444410359));
#14218=CARTESIAN_POINT('',(-1.5595487095344,-2.2,5.59365444410359));
#14219=CARTESIAN_POINT('Origin',(-1.34350288425444,-1.8,5.65649711574556));
#14220=CARTESIAN_POINT('Origin',(-1.34350288425444,-2.2,8.34350288425444));
#14221=CARTESIAN_POINT('',(-1.5595487095344,-2.1,8.40634555589641));
#14222=CARTESIAN_POINT('',(-1.5595487095344,-1.8,8.40634555589641));
#14223=CARTESIAN_POINT('',(-1.5595487095344,-2.2,8.40634555589641));
#14224=CARTESIAN_POINT('',(-1.40634555589641,-2.1,8.5595487095344));
#14225=CARTESIAN_POINT('Origin',(-1.34350288425444,-2.1,8.34350288425444));
#14226=CARTESIAN_POINT('',(-1.40634555589641,-1.8,8.5595487095344));
#14227=CARTESIAN_POINT('',(-1.40634555589641,-2.2,8.5595487095344));
#14228=CARTESIAN_POINT('Origin',(-1.34350288425444,-1.8,8.34350288425444));
#14229=CARTESIAN_POINT('Origin',(1.34350288425444,-2.2,8.34350288425444));
#14230=CARTESIAN_POINT('',(1.40634555589641,-2.1,8.5595487095344));
#14231=CARTESIAN_POINT('',(1.40634555589641,-1.8,8.5595487095344));
#14232=CARTESIAN_POINT('',(1.40634555589641,-2.2,8.5595487095344));
#14233=CARTESIAN_POINT('',(1.5595487095344,-2.1,8.40634555589641));
#14234=CARTESIAN_POINT('Origin',(1.34350288425444,-2.1,8.34350288425444));
#14235=CARTESIAN_POINT('',(1.5595487095344,-1.8,8.40634555589641));
#14236=CARTESIAN_POINT('',(1.5595487095344,-2.2,8.40634555589641));
#14237=CARTESIAN_POINT('Origin',(1.34350288425444,-1.8,8.34350288425444));
#14238=CARTESIAN_POINT('Origin',(1.34350288425444,-2.2,5.65649711574556));
#14239=CARTESIAN_POINT('',(1.5595487095344,-2.1,5.59365444410359));
#14240=CARTESIAN_POINT('',(1.5595487095344,-1.8,5.59365444410359));
#14241=CARTESIAN_POINT('',(1.5595487095344,-2.2,5.59365444410359));
#14242=CARTESIAN_POINT('',(1.40634555589641,-2.1,5.4404512904656));
#14243=CARTESIAN_POINT('Origin',(1.34350288425444,-2.1,5.65649711574556));
#14244=CARTESIAN_POINT('',(1.40634555589641,-1.8,5.4404512904656));
#14245=CARTESIAN_POINT('',(1.40634555589641,-2.2,5.4404512904656));
#14246=CARTESIAN_POINT('Origin',(1.34350288425444,-1.8,5.65649711574556));
#14247=CARTESIAN_POINT('Origin',(0.,-2.1,7.));
#14248=CARTESIAN_POINT('Origin',(0.,-2.1,7.));
#14249=CARTESIAN_POINT('Origin',(0.,-2.1,7.));
#14250=CARTESIAN_POINT('Origin',(0.,-2.1,7.));
#14251=CARTESIAN_POINT('Origin',(0.,-2.1,7.));
#14252=CARTESIAN_POINT('',(-1.1,-2.1,7.));
#14253=CARTESIAN_POINT('Origin',(0.,-2.1,7.));
#14254=CARTESIAN_POINT('Origin',(0.,-2.1,7.));
#14255=CARTESIAN_POINT('Origin',(0.,-1.8,7.));
#14256=CARTESIAN_POINT('Origin',(0.,-2.1,7.));
#14257=CARTESIAN_POINT('Origin',(0.,-1.8,7.));
#14258=CARTESIAN_POINT('Origin',(0.,-2.1,7.));
#14259=CARTESIAN_POINT('Origin',(0.,-1.8,7.));
#14260=CARTESIAN_POINT('Origin',(0.,-2.1,7.));
#14261=CARTESIAN_POINT('Origin',(0.,-1.8,7.));
#14262=CARTESIAN_POINT('Origin',(0.,-1.8,7.));
#14263=CARTESIAN_POINT('',(-1.49,-1.35,7.));
#14264=CARTESIAN_POINT('Origin',(0.,-1.35,7.));
#14265=CARTESIAN_POINT('',(-1.49,-1.8,7.));
#14266=CARTESIAN_POINT('',(-1.49,-1.8,7.));
#14267=CARTESIAN_POINT('Origin',(0.,-1.8,7.));
#14268=CARTESIAN_POINT('Origin',(0.,-1.35,7.));
#14269=CARTESIAN_POINT('',(-1.1,-1.35,7.));
#14270=CARTESIAN_POINT('Origin',(0.,-1.35,7.));
#14271=CARTESIAN_POINT('Origin',(0.,-2.1,7.));
#14272=CARTESIAN_POINT('',(-1.1,-2.1,7.));
#14273=CARTESIAN_POINT('Origin',(0.,-1.8,7.));
#14274=CARTESIAN_POINT('',(0.,0.,0.));
#14275=CARTESIAN_POINT('Origin',(-1.34350288425444,1.7,5.65649711574556));
#14276=CARTESIAN_POINT('',(-1.40634555589641,1.8,5.4404512904656));
#14277=CARTESIAN_POINT('',(-1.40634555589641,2.1,5.4404512904656));
#14278=CARTESIAN_POINT('',(-1.40634555589641,1.7,5.4404512904656));
#14279=CARTESIAN_POINT('',(-1.5595487095344,1.8,5.59365444410359));
#14280=CARTESIAN_POINT('Origin',(-1.34350288425444,1.8,5.65649711574556));
#14281=CARTESIAN_POINT('',(-1.5595487095344,2.1,5.59365444410359));
#14282=CARTESIAN_POINT('',(-1.5595487095344,1.7,5.59365444410359));
#14283=CARTESIAN_POINT('Origin',(-1.34350288425444,2.1,5.65649711574556));
#14284=CARTESIAN_POINT('Origin',(-1.34350288425444,1.7,8.34350288425444));
#14285=CARTESIAN_POINT('',(-1.5595487095344,1.8,8.40634555589641));
#14286=CARTESIAN_POINT('',(-1.5595487095344,2.1,8.40634555589641));
#14287=CARTESIAN_POINT('',(-1.5595487095344,1.7,8.40634555589641));
#14288=CARTESIAN_POINT('',(-1.40634555589641,1.8,8.5595487095344));
#14289=CARTESIAN_POINT('Origin',(-1.34350288425444,1.8,8.34350288425444));
#14290=CARTESIAN_POINT('',(-1.40634555589641,2.1,8.5595487095344));
#14291=CARTESIAN_POINT('',(-1.40634555589641,1.7,8.5595487095344));
#14292=CARTESIAN_POINT('Origin',(-1.34350288425444,2.1,8.34350288425444));
#14293=CARTESIAN_POINT('Origin',(1.34350288425444,1.7,8.34350288425444));
#14294=CARTESIAN_POINT('',(1.40634555589641,1.8,8.5595487095344));
#14295=CARTESIAN_POINT('',(1.40634555589641,2.1,8.5595487095344));
#14296=CARTESIAN_POINT('',(1.40634555589641,1.7,8.5595487095344));
#14297=CARTESIAN_POINT('',(1.5595487095344,1.8,8.40634555589641));
#14298=CARTESIAN_POINT('Origin',(1.34350288425444,1.8,8.34350288425444));
#14299=CARTESIAN_POINT('',(1.5595487095344,2.1,8.40634555589641));
#14300=CARTESIAN_POINT('',(1.5595487095344,1.7,8.40634555589641));
#14301=CARTESIAN_POINT('Origin',(1.34350288425444,2.1,8.34350288425444));
#14302=CARTESIAN_POINT('Origin',(1.34350288425444,1.7,5.65649711574556));
#14303=CARTESIAN_POINT('',(1.5595487095344,1.8,5.59365444410359));
#14304=CARTESIAN_POINT('',(1.5595487095344,2.1,5.59365444410359));
#14305=CARTESIAN_POINT('',(1.5595487095344,1.7,5.59365444410359));
#14306=CARTESIAN_POINT('',(1.40634555589641,1.8,5.4404512904656));
#14307=CARTESIAN_POINT('Origin',(1.34350288425444,1.8,5.65649711574556));
#14308=CARTESIAN_POINT('',(1.40634555589641,2.1,5.4404512904656));
#14309=CARTESIAN_POINT('',(1.40634555589641,1.7,5.4404512904656));
#14310=CARTESIAN_POINT('Origin',(1.34350288425444,2.1,5.65649711574556));
#14311=CARTESIAN_POINT('Origin',(0.,1.8,7.));
#14312=CARTESIAN_POINT('Origin',(0.,1.8,7.));
#14313=CARTESIAN_POINT('Origin',(0.,1.8,7.));
#14314=CARTESIAN_POINT('Origin',(0.,1.8,7.));
#14315=CARTESIAN_POINT('Origin',(0.,1.8,7.));
#14316=CARTESIAN_POINT('',(-1.49,1.8,7.));
#14317=CARTESIAN_POINT('Origin',(0.,1.8,7.));
#14318=CARTESIAN_POINT('Origin',(0.,1.8,7.));
#14319=CARTESIAN_POINT('Origin',(0.,2.1,7.));
#14320=CARTESIAN_POINT('Origin',(0.,1.8,7.));
#14321=CARTESIAN_POINT('Origin',(0.,2.1,7.));
#14322=CARTESIAN_POINT('Origin',(0.,1.8,7.));
#14323=CARTESIAN_POINT('Origin',(0.,2.1,7.));
#14324=CARTESIAN_POINT('Origin',(0.,1.8,7.));
#14325=CARTESIAN_POINT('Origin',(0.,2.1,7.));
#14326=CARTESIAN_POINT('Origin',(0.,1.35,7.));
#14327=CARTESIAN_POINT('',(-1.49,1.35,7.));
#14328=CARTESIAN_POINT('',(-1.49,1.35,7.));
#14329=CARTESIAN_POINT('Origin',(0.,1.35,7.));
#14330=CARTESIAN_POINT('Origin',(0.,1.35,7.));
#14331=CARTESIAN_POINT('',(-1.1,1.35,7.));
#14332=CARTESIAN_POINT('Origin',(0.,1.35,7.));
#14333=CARTESIAN_POINT('Origin',(0.,1.8,7.));
#14334=CARTESIAN_POINT('',(-1.1,2.1,7.));
#14335=CARTESIAN_POINT('Origin',(0.,2.1,7.));
#14336=CARTESIAN_POINT('',(-1.1,1.8,7.));
#14337=CARTESIAN_POINT('Origin',(0.,2.1,7.));
#14338=CARTESIAN_POINT('',(0.,0.,0.));
#14339=CARTESIAN_POINT('Origin',(5.55669646780806,-1.9,5.58578643762691));
#14340=CARTESIAN_POINT('',(5.39169646780806,-1.8,5.58578643762691));
#14341=CARTESIAN_POINT('Origin',(5.55669646780806,-1.8,5.58578643762691));
#14342=CARTESIAN_POINT('',(5.39169646780806,1.8,5.58578643762691));
#14343=CARTESIAN_POINT('',(5.39169646780806,-1.9,5.58578643762691));
#14344=CARTESIAN_POINT('Origin',(5.55669646780806,1.8,5.58578643762691));
#14345=CARTESIAN_POINT('Origin',(5.55669646780806,-1.9,8.4142135623731));
#14346=CARTESIAN_POINT('',(5.39169646780806,-1.8,8.4142135623731));
#14347=CARTESIAN_POINT('Origin',(5.55669646780806,-1.8,8.4142135623731));
#14348=CARTESIAN_POINT('',(5.39169646780806,1.8,8.4142135623731));
#14349=CARTESIAN_POINT('',(5.39169646780806,-1.9,8.4142135623731));
#14350=CARTESIAN_POINT('Origin',(5.55669646780806,1.8,8.4142135623731));
#14351=CARTESIAN_POINT('Origin',(8.38512359255425,-1.9,8.4142135623731));
#14352=CARTESIAN_POINT('',(8.22012359255425,-1.8,8.4142135623731));
#14353=CARTESIAN_POINT('Origin',(8.38512359255425,-1.8,8.4142135623731));
#14354=CARTESIAN_POINT('',(8.22012359255425,1.8,8.4142135623731));
#14355=CARTESIAN_POINT('',(8.22012359255425,-1.9,8.4142135623731));
#14356=CARTESIAN_POINT('Origin',(8.38512359255425,1.8,8.4142135623731));
#14357=CARTESIAN_POINT('Origin',(8.38512359255425,-1.9,5.58578643762691));
#14358=CARTESIAN_POINT('',(8.22012359255425,-1.8,5.58578643762691));
#14359=CARTESIAN_POINT('Origin',(8.38512359255425,-1.8,5.58578643762691));
#14360=CARTESIAN_POINT('',(8.22012359255425,1.8,5.58578643762691));
#14361=CARTESIAN_POINT('',(8.22012359255425,-1.9,5.58578643762691));
#14362=CARTESIAN_POINT('Origin',(8.38512359255425,1.8,5.58578643762691));
#14363=CARTESIAN_POINT('Origin',(6.97091003018116,-1.9,7.));
#14364=CARTESIAN_POINT('',(5.37091003018116,-1.8,7.));
#14365=CARTESIAN_POINT('Origin',(6.97091003018116,-1.8,7.));
#14366=CARTESIAN_POINT('',(5.37091003018116,1.8,7.));
#14367=CARTESIAN_POINT('',(5.37091003018116,-1.9,7.));
#14368=CARTESIAN_POINT('Origin',(6.97091003018116,1.8,7.));
#14369=CARTESIAN_POINT('Origin',(9.77091003018116,-1.,-0.1));
#14370=CARTESIAN_POINT('',(9.54591003018116,-1.,0.));
#14371=CARTESIAN_POINT('Origin',(9.77091003018116,-1.,0.));
#14372=CARTESIAN_POINT('',(9.54591003018116,-1.,0.8));
#14373=CARTESIAN_POINT('',(9.54591003018116,-1.,-0.1));
#14374=CARTESIAN_POINT('Origin',(9.77091003018116,-1.,0.8));
#14375=CARTESIAN_POINT('Origin',(4.17091003018116,1.,-0.1));
#14376=CARTESIAN_POINT('',(3.94591003018116,1.,0.));
#14377=CARTESIAN_POINT('Origin',(4.17091003018116,1.,0.));
#14378=CARTESIAN_POINT('',(3.94591003018116,1.,0.8));
#14379=CARTESIAN_POINT('',(3.94591003018116,1.,-0.1));
#14380=CARTESIAN_POINT('Origin',(4.17091003018116,1.,0.8));
#14381=CARTESIAN_POINT('Origin',(4.17091003018116,-1.,-0.1));
#14382=CARTESIAN_POINT('',(3.94591003018116,-1.,0.));
#14383=CARTESIAN_POINT('Origin',(4.17091003018116,-1.,0.));
#14384=CARTESIAN_POINT('',(3.94591003018116,-1.,0.8));
#14385=CARTESIAN_POINT('',(3.94591003018116,-1.,-0.1));
#14386=CARTESIAN_POINT('Origin',(4.17091003018116,-1.,0.8));
#14387=CARTESIAN_POINT('Origin',(9.77091003018116,1.,-0.1));
#14388=CARTESIAN_POINT('',(9.54591003018116,1.,0.));
#14389=CARTESIAN_POINT('Origin',(9.77091003018116,1.,0.));
#14390=CARTESIAN_POINT('',(9.54591003018116,1.,0.8));
#14391=CARTESIAN_POINT('',(9.54591003018116,1.,-0.1));
#14392=CARTESIAN_POINT('Origin',(9.77091003018116,1.,0.8));
#14393=CARTESIAN_POINT('Origin',(3.57091003018116,-1.8,0.8));
#14394=CARTESIAN_POINT('',(9.17091003018116,-1.8,0.8));
#14395=CARTESIAN_POINT('',(9.17091003018116,1.8,0.8));
#14396=CARTESIAN_POINT('',(9.17091003018116,-1.8,0.8));
#14397=CARTESIAN_POINT('',(10.3709100301812,-1.8,0.8));
#14398=CARTESIAN_POINT('',(10.3709100301812,-1.8,0.8));
#14399=CARTESIAN_POINT('',(10.3709100301812,1.8,0.8));
#14400=CARTESIAN_POINT('',(10.3709100301812,-1.8,0.8));
#14401=CARTESIAN_POINT('',(10.3709100301812,1.8,0.8));
#14402=CARTESIAN_POINT('Origin',(3.57091003018116,-1.8,0.8));
#14403=CARTESIAN_POINT('',(4.77091003018116,1.8,0.8));
#14404=CARTESIAN_POINT('',(4.77091003018116,-1.8,0.8));
#14405=CARTESIAN_POINT('',(4.77091003018116,0.,0.8));
#14406=CARTESIAN_POINT('',(3.57091003018116,1.8,0.8));
#14407=CARTESIAN_POINT('',(10.3709100301812,1.8,0.8));
#14408=CARTESIAN_POINT('',(3.57091003018116,-1.8,0.8));
#14409=CARTESIAN_POINT('',(3.57091003018116,-1.8,0.8));
#14410=CARTESIAN_POINT('',(10.3709100301812,-1.8,0.8));
#14411=CARTESIAN_POINT('Origin',(3.57091003018116,-1.8,0.));
#14412=CARTESIAN_POINT('',(3.57091003018116,-1.8,0.));
#14413=CARTESIAN_POINT('',(3.57091003018116,-1.8,0.8));
#14414=CARTESIAN_POINT('',(3.57091003018116,1.8,0.));
#14415=CARTESIAN_POINT('',(3.57091003018116,1.8,0.8));
#14416=CARTESIAN_POINT('',(3.57091003018116,-1.8,0.));
#14417=CARTESIAN_POINT('Origin',(10.3709100301812,-1.8,0.8));
#14418=CARTESIAN_POINT('',(10.3709100301812,-1.8,0.));
#14419=CARTESIAN_POINT('',(10.3709100301812,-1.8,0.));
#14420=CARTESIAN_POINT('',(10.3709100301812,1.8,0.));
#14421=CARTESIAN_POINT('',(10.3709100301812,-1.8,0.));
#14422=CARTESIAN_POINT('',(10.3709100301812,1.8,0.));
#14423=CARTESIAN_POINT('Origin',(4.77091003018116,-1.8,0.));
#14424=CARTESIAN_POINT('',(9.17091003018116,-1.8,9.2));
#14425=CARTESIAN_POINT('',(9.17091003018116,-1.8,0.));
#14426=CARTESIAN_POINT('',(4.77091003018116,-1.8,9.2));
#14427=CARTESIAN_POINT('',(4.77091003018116,-1.8,9.2));
#14428=CARTESIAN_POINT('',(4.77091003018116,-1.8,0.));
#14429=CARTESIAN_POINT('',(3.57091003018116,-1.8,0.));
#14430=CARTESIAN_POINT('Origin',(9.17091003018116,-1.8,0.));
#14431=CARTESIAN_POINT('',(9.17091003018116,1.8,9.2));
#14432=CARTESIAN_POINT('',(9.17091003018116,1.8,0.));
#14433=CARTESIAN_POINT('',(9.17091003018116,-1.8,9.2));
#14434=CARTESIAN_POINT('Origin',(9.17091003018116,1.8,0.));
#14435=CARTESIAN_POINT('',(4.77091003018116,1.8,9.2));
#14436=CARTESIAN_POINT('',(4.77091003018116,1.8,0.));
#14437=CARTESIAN_POINT('',(9.17091003018116,1.8,9.2));
#14438=CARTESIAN_POINT('',(3.57091003018116,1.8,0.));
#14439=CARTESIAN_POINT('Origin',(4.77091003018116,1.8,0.));
#14440=CARTESIAN_POINT('',(4.77091003018116,1.8,9.2));
#14441=CARTESIAN_POINT('Origin',(6.97091003018116,0.,9.2));
#14442=CARTESIAN_POINT('Origin',(6.97091003018116,0.,0.));
#14443=CARTESIAN_POINT('',(0.,0.,0.));
#14444=CARTESIAN_POINT('Origin',(4.17091003018116,-1.,-1.6));
#14445=CARTESIAN_POINT('',(4.00591003018116,-1.,-1.2));
#14446=CARTESIAN_POINT('Origin',(4.17091003018116,-1.,-1.2));
#14447=CARTESIAN_POINT('',(4.00591003018116,-1.,-1.6));
#14448=CARTESIAN_POINT('',(4.00591003018116,-1.,-1.6));
#14449=CARTESIAN_POINT('Origin',(4.17091003018116,-1.,-1.6));
#14450=CARTESIAN_POINT('Origin',(4.17091003018116,-1.,-1.6));
#14451=CARTESIAN_POINT('',(3.77091003018116,-1.,-1.2));
#14452=CARTESIAN_POINT('Origin',(4.17091003018116,-1.,-1.2));
#14453=CARTESIAN_POINT('',(3.77091003018116,-1.,-1.6));
#14454=CARTESIAN_POINT('',(3.77091003018116,-1.,-1.6));
#14455=CARTESIAN_POINT('Origin',(4.17091003018116,-1.,-1.6));
#14456=CARTESIAN_POINT('Origin',(4.17091003018116,-1.,-1.2));
#14457=CARTESIAN_POINT('Origin',(4.17091003018116,-1.,-1.6));
#14458=CARTESIAN_POINT('',(0.,0.,0.));
#14459=CARTESIAN_POINT('Origin',(4.17091003018116,1.,-1.6));
#14460=CARTESIAN_POINT('',(4.00591003018116,1.,-1.2));
#14461=CARTESIAN_POINT('Origin',(4.17091003018116,1.,-1.2));
#14462=CARTESIAN_POINT('',(4.00591003018116,1.,-1.6));
#14463=CARTESIAN_POINT('',(4.00591003018116,1.,-1.6));
#14464=CARTESIAN_POINT('Origin',(4.17091003018116,1.,-1.6));
#14465=CARTESIAN_POINT('Origin',(4.17091003018116,1.,-1.6));
#14466=CARTESIAN_POINT('',(3.77091003018116,1.,-1.2));
#14467=CARTESIAN_POINT('Origin',(4.17091003018116,1.,-1.2));
#14468=CARTESIAN_POINT('',(3.77091003018116,1.,-1.6));
#14469=CARTESIAN_POINT('',(3.77091003018116,1.,-1.6));
#14470=CARTESIAN_POINT('Origin',(4.17091003018116,1.,-1.6));
#14471=CARTESIAN_POINT('Origin',(4.17091003018116,1.,-1.2));
#14472=CARTESIAN_POINT('Origin',(4.17091003018116,1.,-1.6));
#14473=CARTESIAN_POINT('',(0.,0.,0.));
#14474=CARTESIAN_POINT('Origin',(9.77091003018116,-1.,-1.6));
#14475=CARTESIAN_POINT('',(9.60591003018116,-1.,-1.2));
#14476=CARTESIAN_POINT('Origin',(9.77091003018116,-1.,-1.2));
#14477=CARTESIAN_POINT('',(9.60591003018116,-1.,-1.6));
#14478=CARTESIAN_POINT('',(9.60591003018116,-1.,-1.6));
#14479=CARTESIAN_POINT('Origin',(9.77091003018116,-1.,-1.6));
#14480=CARTESIAN_POINT('Origin',(9.77091003018116,-1.,-1.6));
#14481=CARTESIAN_POINT('',(9.37091003018116,-1.,-1.2));
#14482=CARTESIAN_POINT('Origin',(9.77091003018116,-1.,-1.2));
#14483=CARTESIAN_POINT('',(9.37091003018116,-1.,-1.6));
#14484=CARTESIAN_POINT('',(9.37091003018116,-1.,-1.6));
#14485=CARTESIAN_POINT('Origin',(9.77091003018116,-1.,-1.6));
#14486=CARTESIAN_POINT('Origin',(9.77091003018116,-1.,-1.2));
#14487=CARTESIAN_POINT('Origin',(9.77091003018116,-1.,-1.6));
#14488=CARTESIAN_POINT('',(0.,0.,0.));
#14489=CARTESIAN_POINT('Origin',(9.77091003018116,1.,-1.6));
#14490=CARTESIAN_POINT('',(9.60591003018116,1.,-1.2));
#14491=CARTESIAN_POINT('Origin',(9.77091003018116,1.,-1.2));
#14492=CARTESIAN_POINT('',(9.60591003018116,1.,-1.6));
#14493=CARTESIAN_POINT('',(9.60591003018116,1.,-1.6));
#14494=CARTESIAN_POINT('Origin',(9.77091003018116,1.,-1.6));
#14495=CARTESIAN_POINT('Origin',(9.77091003018116,1.,-1.6));
#14496=CARTESIAN_POINT('',(9.37091003018116,1.,-1.2));
#14497=CARTESIAN_POINT('Origin',(9.77091003018116,1.,-1.2));
#14498=CARTESIAN_POINT('',(9.37091003018116,1.,-1.6));
#14499=CARTESIAN_POINT('',(9.37091003018116,1.,-1.6));
#14500=CARTESIAN_POINT('Origin',(9.77091003018116,1.,-1.6));
#14501=CARTESIAN_POINT('Origin',(9.77091003018116,1.,-1.2));
#14502=CARTESIAN_POINT('Origin',(9.77091003018116,1.,-1.6));
#14503=CARTESIAN_POINT('',(0.,0.,0.));
#14504=CARTESIAN_POINT('Origin',(6.97091003018116,-0.4,7.));
#14505=CARTESIAN_POINT('',(5.77091003018116,0.4,7.));
#14506=CARTESIAN_POINT('Origin',(6.97091003018116,0.4,7.));
#14507=CARTESIAN_POINT('',(5.77091003018116,-0.4,7.));
#14508=CARTESIAN_POINT('',(5.77091003018116,-0.4,7.));
#14509=CARTESIAN_POINT('Origin',(6.97091003018116,-0.4,7.));
#14510=CARTESIAN_POINT('Origin',(6.97091003018116,-0.4,7.));
#14511=CARTESIAN_POINT('',(5.38091003018116,0.4,7.));
#14512=CARTESIAN_POINT('Origin',(6.97091003018116,0.4,7.));
#14513=CARTESIAN_POINT('',(5.38091003018116,-0.4,7.));
#14514=CARTESIAN_POINT('',(5.38091003018116,-0.4,7.));
#14515=CARTESIAN_POINT('Origin',(6.97091003018116,-0.4,7.));
#14516=CARTESIAN_POINT('Origin',(6.97091003018116,0.4,7.));
#14517=CARTESIAN_POINT('Origin',(6.97091003018116,-0.4,7.));
#14518=CARTESIAN_POINT('',(0.,0.,0.));
#14519=CARTESIAN_POINT('Origin',(5.55669646780806,-2.2,5.58578643762691));
#14520=CARTESIAN_POINT('',(5.49357471024299,-2.1,5.36982198749241));
#14521=CARTESIAN_POINT('',(5.49357471024299,-1.8,5.36982198749241));
#14522=CARTESIAN_POINT('',(5.49357471024299,-2.2,5.36982198749241));
#14523=CARTESIAN_POINT('',(5.34073201767356,-2.1,5.52266468006184));
#14524=CARTESIAN_POINT('Origin',(5.55669646780806,-2.1,5.58578643762691));
#14525=CARTESIAN_POINT('',(5.34073201767356,-1.8,5.52266468006184));
#14526=CARTESIAN_POINT('',(5.34073201767356,-2.2,5.52266468006184));
#14527=CARTESIAN_POINT('Origin',(5.55669646780806,-1.8,5.58578643762691));
#14528=CARTESIAN_POINT('Origin',(5.55669646780806,-2.2,8.4142135623731));
#14529=CARTESIAN_POINT('',(5.34073201767356,-2.1,8.47733531993816));
#14530=CARTESIAN_POINT('',(5.34073201767356,-1.8,8.47733531993816));
#14531=CARTESIAN_POINT('',(5.34073201767356,-2.2,8.47733531993816));
#14532=CARTESIAN_POINT('',(5.493574710243,-2.1,8.6301780125076));
#14533=CARTESIAN_POINT('Origin',(5.55669646780806,-2.1,8.4142135623731));
#14534=CARTESIAN_POINT('',(5.493574710243,-1.8,8.6301780125076));
#14535=CARTESIAN_POINT('',(5.493574710243,-2.2,8.6301780125076));
#14536=CARTESIAN_POINT('Origin',(5.55669646780806,-1.8,8.4142135623731));
#14537=CARTESIAN_POINT('Origin',(8.38512359255425,-2.2,8.4142135623731));
#14538=CARTESIAN_POINT('',(8.44824535011931,-2.1,8.6301780125076));
#14539=CARTESIAN_POINT('',(8.44824535011931,-1.8,8.6301780125076));
#14540=CARTESIAN_POINT('',(8.44824535011932,-2.2,8.6301780125076));
#14541=CARTESIAN_POINT('',(8.60108804268875,-2.1,8.47733531993816));
#14542=CARTESIAN_POINT('Origin',(8.38512359255425,-2.1,8.4142135623731));
#14543=CARTESIAN_POINT('',(8.60108804268875,-1.8,8.47733531993816));
#14544=CARTESIAN_POINT('',(8.60108804268875,-2.2,8.47733531993816));
#14545=CARTESIAN_POINT('Origin',(8.38512359255425,-1.8,8.4142135623731));
#14546=CARTESIAN_POINT('Origin',(8.38512359255425,-2.2,5.58578643762691));
#14547=CARTESIAN_POINT('',(8.60108804268875,-2.1,5.52266468006184));
#14548=CARTESIAN_POINT('',(8.60108804268875,-1.8,5.52266468006184));
#14549=CARTESIAN_POINT('',(8.60108804268875,-2.2,5.52266468006184));
#14550=CARTESIAN_POINT('',(8.44824535011932,-2.1,5.36982198749241));
#14551=CARTESIAN_POINT('Origin',(8.38512359255425,-2.1,5.58578643762691));
#14552=CARTESIAN_POINT('',(8.44824535011932,-1.8,5.36982198749241));
#14553=CARTESIAN_POINT('',(8.44824535011932,-2.2,5.36982198749241));
#14554=CARTESIAN_POINT('Origin',(8.38512359255425,-1.8,5.58578643762691));
#14555=CARTESIAN_POINT('Origin',(6.97091003018116,-2.1,7.));
#14556=CARTESIAN_POINT('Origin',(6.97091003018116,-2.1,7.));
#14557=CARTESIAN_POINT('Origin',(6.97091003018116,-2.1,7.));
#14558=CARTESIAN_POINT('Origin',(6.97091003018116,-2.1,7.));
#14559=CARTESIAN_POINT('Origin',(6.97091003018116,-2.1,7.));
#14560=CARTESIAN_POINT('',(5.77091003018116,-2.1,7.));
#14561=CARTESIAN_POINT('Origin',(6.97091003018116,-2.1,7.));
#14562=CARTESIAN_POINT('Origin',(6.97091003018116,-2.1,7.));
#14563=CARTESIAN_POINT('Origin',(6.97091003018116,-1.8,7.));
#14564=CARTESIAN_POINT('Origin',(6.97091003018116,-2.1,7.));
#14565=CARTESIAN_POINT('Origin',(6.97091003018116,-1.8,7.));
#14566=CARTESIAN_POINT('Origin',(6.97091003018116,-2.1,7.));
#14567=CARTESIAN_POINT('Origin',(6.97091003018116,-1.8,7.));
#14568=CARTESIAN_POINT('Origin',(6.97091003018116,-2.1,7.));
#14569=CARTESIAN_POINT('Origin',(6.97091003018116,-1.8,7.));
#14570=CARTESIAN_POINT('Origin',(6.97091003018116,-1.8,7.));
#14571=CARTESIAN_POINT('',(5.38091003018116,-1.4,7.));
#14572=CARTESIAN_POINT('Origin',(6.97091003018116,-1.4,7.));
#14573=CARTESIAN_POINT('',(5.38091003018116,-1.8,7.));
#14574=CARTESIAN_POINT('',(5.38091003018116,-1.8,7.));
#14575=CARTESIAN_POINT('Origin',(6.97091003018116,-1.8,7.));
#14576=CARTESIAN_POINT('Origin',(6.97091003018116,-1.4,7.));
#14577=CARTESIAN_POINT('',(5.77091003018116,-1.4,7.));
#14578=CARTESIAN_POINT('Origin',(6.97091003018116,-1.4,7.));
#14579=CARTESIAN_POINT('Origin',(6.97091003018116,-2.1,7.));
#14580=CARTESIAN_POINT('',(5.77091003018116,-2.1,7.));
#14581=CARTESIAN_POINT('Origin',(6.97091003018116,-1.8,7.));
#14582=CARTESIAN_POINT('',(0.,0.,0.));
#14583=CARTESIAN_POINT('Origin',(5.55669646780806,1.7,5.58578643762691));
#14584=CARTESIAN_POINT('',(5.49357471024299,1.8,5.36982198749241));
#14585=CARTESIAN_POINT('',(5.49357471024299,2.1,5.36982198749241));
#14586=CARTESIAN_POINT('',(5.49357471024299,1.7,5.36982198749241));
#14587=CARTESIAN_POINT('',(5.34073201767356,1.8,5.52266468006184));
#14588=CARTESIAN_POINT('Origin',(5.55669646780806,1.8,5.58578643762691));
#14589=CARTESIAN_POINT('',(5.34073201767356,2.1,5.52266468006184));
#14590=CARTESIAN_POINT('',(5.34073201767356,1.7,5.52266468006184));
#14591=CARTESIAN_POINT('Origin',(5.55669646780806,2.1,5.58578643762691));
#14592=CARTESIAN_POINT('Origin',(5.55669646780806,1.7,8.4142135623731));
#14593=CARTESIAN_POINT('',(5.34073201767356,1.8,8.47733531993816));
#14594=CARTESIAN_POINT('',(5.34073201767356,2.1,8.47733531993816));
#14595=CARTESIAN_POINT('',(5.34073201767356,1.7,8.47733531993816));
#14596=CARTESIAN_POINT('',(5.493574710243,1.8,8.6301780125076));
#14597=CARTESIAN_POINT('Origin',(5.55669646780806,1.8,8.4142135623731));
#14598=CARTESIAN_POINT('',(5.493574710243,2.1,8.6301780125076));
#14599=CARTESIAN_POINT('',(5.493574710243,1.7,8.6301780125076));
#14600=CARTESIAN_POINT('Origin',(5.55669646780806,2.1,8.4142135623731));
#14601=CARTESIAN_POINT('Origin',(8.38512359255425,1.7,8.4142135623731));
#14602=CARTESIAN_POINT('',(8.44824535011931,1.8,8.6301780125076));
#14603=CARTESIAN_POINT('',(8.44824535011931,2.1,8.6301780125076));
#14604=CARTESIAN_POINT('',(8.44824535011932,1.7,8.6301780125076));
#14605=CARTESIAN_POINT('',(8.60108804268875,1.8,8.47733531993816));
#14606=CARTESIAN_POINT('Origin',(8.38512359255425,1.8,8.4142135623731));
#14607=CARTESIAN_POINT('',(8.60108804268875,2.1,8.47733531993816));
#14608=CARTESIAN_POINT('',(8.60108804268875,1.7,8.47733531993816));
#14609=CARTESIAN_POINT('Origin',(8.38512359255425,2.1,8.4142135623731));
#14610=CARTESIAN_POINT('Origin',(8.38512359255425,1.7,5.58578643762691));
#14611=CARTESIAN_POINT('',(8.60108804268875,1.8,5.52266468006184));
#14612=CARTESIAN_POINT('',(8.60108804268875,2.1,5.52266468006184));
#14613=CARTESIAN_POINT('',(8.60108804268875,1.7,5.52266468006184));
#14614=CARTESIAN_POINT('',(8.44824535011932,1.8,5.36982198749241));
#14615=CARTESIAN_POINT('Origin',(8.38512359255425,1.8,5.58578643762691));
#14616=CARTESIAN_POINT('',(8.44824535011932,2.1,5.36982198749241));
#14617=CARTESIAN_POINT('',(8.44824535011932,1.7,5.36982198749241));
#14618=CARTESIAN_POINT('Origin',(8.38512359255425,2.1,5.58578643762691));
#14619=CARTESIAN_POINT('Origin',(6.97091003018116,1.8,7.));
#14620=CARTESIAN_POINT('Origin',(6.97091003018116,1.8,7.));
#14621=CARTESIAN_POINT('Origin',(6.97091003018116,1.8,7.));
#14622=CARTESIAN_POINT('Origin',(6.97091003018116,1.8,7.));
#14623=CARTESIAN_POINT('Origin',(6.97091003018116,1.8,7.));
#14624=CARTESIAN_POINT('',(5.38091003018116,1.8,7.));
#14625=CARTESIAN_POINT('Origin',(6.97091003018116,1.8,7.));
#14626=CARTESIAN_POINT('Origin',(6.97091003018116,1.8,7.));
#14627=CARTESIAN_POINT('Origin',(6.97091003018116,2.1,7.));
#14628=CARTESIAN_POINT('Origin',(6.97091003018116,1.8,7.));
#14629=CARTESIAN_POINT('Origin',(6.97091003018116,2.1,7.));
#14630=CARTESIAN_POINT('Origin',(6.97091003018116,1.8,7.));
#14631=CARTESIAN_POINT('Origin',(6.97091003018116,2.1,7.));
#14632=CARTESIAN_POINT('Origin',(6.97091003018116,1.8,7.));
#14633=CARTESIAN_POINT('Origin',(6.97091003018116,2.1,7.));
#14634=CARTESIAN_POINT('Origin',(6.97091003018116,1.4,7.));
#14635=CARTESIAN_POINT('',(5.38091003018116,1.4,7.));
#14636=CARTESIAN_POINT('',(5.38091003018116,1.4,7.));
#14637=CARTESIAN_POINT('Origin',(6.97091003018116,1.4,7.));
#14638=CARTESIAN_POINT('Origin',(6.97091003018116,1.4,7.));
#14639=CARTESIAN_POINT('',(5.77091003018116,1.4,7.));
#14640=CARTESIAN_POINT('Origin',(6.97091003018116,1.4,7.));
#14641=CARTESIAN_POINT('Origin',(6.97091003018116,1.8,7.));
#14642=CARTESIAN_POINT('',(5.77091003018116,2.1,7.));
#14643=CARTESIAN_POINT('Origin',(6.97091003018116,2.1,7.));
#14644=CARTESIAN_POINT('',(5.77091003018116,1.8,7.));
#14645=CARTESIAN_POINT('Origin',(6.97091003018116,2.1,7.));
#14646=CARTESIAN_POINT('',(0.,0.,0.));
#14647=CARTESIAN_POINT('Origin',(6.85463117051588,-3.5,5.73208116779017));
#14648=CARTESIAN_POINT('',(6.85463117051588,-3.425,5.73208116779017));
#14649=CARTESIAN_POINT('',(-0.0581394298326381,-3.425,6.36604058389508));
#14650=CARTESIAN_POINT('',(3.39824587034162,-3.425,6.04906087584262));
#14651=CARTESIAN_POINT('',(6.85463117051588,-2.825,5.73208116779017));
#14652=CARTESIAN_POINT('',(6.85463117051588,-3.5,5.73208116779017));
#14653=CARTESIAN_POINT('',(-0.0581394298326381,-2.825,6.36604058389508));
#14654=CARTESIAN_POINT('',(3.39824587034162,-2.825,6.04906087584262));
#14655=CARTESIAN_POINT('',(-0.0581394298326381,-3.5,6.36604058389508));
#14656=CARTESIAN_POINT('Origin',(-0.0581394298326382,-3.5,7.63395941610492));
#14657=CARTESIAN_POINT('',(-0.0581394298326382,-3.425,7.63395941610492));
#14658=CARTESIAN_POINT('',(6.85463117051588,-3.425,8.26791883220983));
#14659=CARTESIAN_POINT('',(-0.0581394298326382,-3.425,7.63395941610492));
#14660=CARTESIAN_POINT('',(-0.0581394298326382,-2.825,7.63395941610492));
#14661=CARTESIAN_POINT('',(-0.0581394298326382,-3.5,7.63395941610492));
#14662=CARTESIAN_POINT('',(6.85463117051588,-2.825,8.26791883220983));
#14663=CARTESIAN_POINT('',(-0.0581394298326382,-2.825,7.63395941610492));
#14664=CARTESIAN_POINT('',(6.85463117051588,-3.5,8.26791883220983));
#14665=CARTESIAN_POINT('Origin',(0.,-3.425,7.));
#14666=CARTESIAN_POINT('',(-0.067271950114944,-3.425,7.73354152832038));
#14667=CARTESIAN_POINT('',(6.84549865023357,-3.425,8.3675009444253));
#14668=CARTESIAN_POINT('',(-0.067271950114944,-3.425,7.73354152832038));
#14669=CARTESIAN_POINT('',(-0.067271950114944,-3.425,6.26645847167962));
#14670=CARTESIAN_POINT('Origin',(0.,-3.425,7.));
#14671=CARTESIAN_POINT('',(6.84549865023357,-3.425,5.6324990555747));
#14672=CARTESIAN_POINT('',(6.84549865023357,-3.425,5.6324990555747));
#14673=CARTESIAN_POINT('Origin',(6.97091003018116,-3.425,7.));
#14674=CARTESIAN_POINT('Origin',(0.,-3.425,7.));
#14675=CARTESIAN_POINT('Origin',(6.97091003018116,-3.425,7.));
#14676=CARTESIAN_POINT('Origin',(0.,-3.5,7.));
#14677=CARTESIAN_POINT('Origin',(0.,-2.825,7.));
#14678=CARTESIAN_POINT('Origin',(6.97091003018116,-3.5,7.));
#14679=CARTESIAN_POINT('Origin',(6.97091003018116,-2.825,7.));
#14680=CARTESIAN_POINT('Origin',(6.97091003018116,-3.425,7.));
#14681=CARTESIAN_POINT('',(6.84549865023357,-2.825,5.6324990555747));
#14682=CARTESIAN_POINT('',(6.84549865023357,-3.425,5.6324990555747));
#14683=CARTESIAN_POINT('',(6.84549865023357,-2.825,8.3675009444253));
#14684=CARTESIAN_POINT('Origin',(6.97091003018116,-2.825,7.));
#14685=CARTESIAN_POINT('',(6.84549865023357,-3.425,8.3675009444253));
#14686=CARTESIAN_POINT('Origin',(6.84549865023357,-3.425,5.6324990555747));
#14687=CARTESIAN_POINT('',(-0.067271950114944,-2.825,6.26645847167962));
#14688=CARTESIAN_POINT('',(-0.0672719501149439,-3.425,6.26645847167962));
#14689=CARTESIAN_POINT('',(6.84549865023357,-2.825,5.6324990555747));
#14690=CARTESIAN_POINT('Origin',(-0.067271950114944,-3.425,7.73354152832038));
#14691=CARTESIAN_POINT('',(-0.067271950114944,-2.825,7.73354152832038));
#14692=CARTESIAN_POINT('',(-0.067271950114944,-2.825,7.73354152832038));
#14693=CARTESIAN_POINT('',(-0.0672719501149441,-3.425,7.73354152832038));
#14694=CARTESIAN_POINT('Origin',(0.,-3.425,7.));
#14695=CARTESIAN_POINT('Origin',(0.,-2.825,7.));
#14696=CARTESIAN_POINT('Origin',(0.,-2.825,7.));
#14697=CARTESIAN_POINT('',(0.,0.,0.));
#14698=CARTESIAN_POINT('',(0.,0.,0.));
#14699=CARTESIAN_POINT('Origin',(0.,0.,0.));
#14700=CARTESIAN_POINT('',(-0.976185,-0.246528389340863,-1.19548183562566E-16));
#14701=CARTESIAN_POINT('',(-1.19548183562566E-16,-0.246528389340863,0.976185));
#14702=CARTESIAN_POINT('Origin',(0.,-0.246528389340863,0.));
#14703=CARTESIAN_POINT('Origin',(0.,-0.246528389340863,0.));
#14704=CARTESIAN_POINT('',(-1.19548183562566E-16,0.246528389340863,0.976185));
#14705=CARTESIAN_POINT('Origin',(-1.22464679914735E-16,0.,1.));
#14706=CARTESIAN_POINT('',(-0.976185,0.246528389340863,1.19548183562566E-16));
#14707=CARTESIAN_POINT('Origin',(0.,0.246528389340863,0.));
#14708=CARTESIAN_POINT('Origin',(0.,0.246528389340863,0.));
#14709=CARTESIAN_POINT('Origin',(0.,0.,0.));
#14710=CARTESIAN_POINT('',(-0.976185,0.45,-1.19548183562566E-16));
#14711=CARTESIAN_POINT('',(-0.976185,0.,-1.19548183562566E-16));
#14712=CARTESIAN_POINT('Origin',(0.,0.45,0.));
#14713=CARTESIAN_POINT('Origin',(0.,0.,0.));
#14714=CARTESIAN_POINT('',(-0.5,-0.39,-6.12323399573677E-17));
#14715=CARTESIAN_POINT('Origin',(0.,-0.39,0.));
#14716=CARTESIAN_POINT('',(-0.5,0.39,-6.12323399573677E-17));
#14717=CARTESIAN_POINT('',(-0.5,0.,-6.12323399573677E-17));
#14718=CARTESIAN_POINT('Origin',(0.,0.39,0.));
#14719=CARTESIAN_POINT('Origin',(0.,0.42,0.));
#14720=CARTESIAN_POINT('',(-0.56,0.45,-6.85802207522518E-17));
#14721=CARTESIAN_POINT('',(-0.53,0.42,-6.49062803548097E-17));
#14722=CARTESIAN_POINT('Origin',(0.,0.45,0.));
#14723=CARTESIAN_POINT('Origin',(0.976185,0.45,0.));
#14724=CARTESIAN_POINT('Origin',(0.,0.,0.));
#14725=CARTESIAN_POINT('',(-0.976185,-0.45,-1.19548183562566E-16));
#14726=CARTESIAN_POINT('Origin',(0.,-0.45,0.));
#14727=CARTESIAN_POINT('',(-0.976185,0.,-1.19548183562566E-16));
#14728=CARTESIAN_POINT('Origin',(0.56,-0.45,0.));
#14729=CARTESIAN_POINT('',(-0.56,-0.45,-6.85802207522518E-17));
#14730=CARTESIAN_POINT('Origin',(0.,-0.45,0.));
#14731=CARTESIAN_POINT('Origin',(0.,-0.42,0.));
#14732=CARTESIAN_POINT('',(-0.53,-0.42,-6.49062803548097E-17));
#14733=CARTESIAN_POINT('',(0.,0.,0.));
#14734=CARTESIAN_POINT('Origin',(0.,0.,0.));
#14735=CARTESIAN_POINT('',(-1.023815,0.246528389340863,-1.25381176266905E-16));
#14736=CARTESIAN_POINT('',(-1.25381176266905E-16,0.246528389340863,1.023815));
#14737=CARTESIAN_POINT('Origin',(0.,0.246528389340863,0.));
#14738=CARTESIAN_POINT('Origin',(0.,0.246528389340863,0.));
#14739=CARTESIAN_POINT('',(-1.25381176266905E-16,-0.246528389340863,1.023815));
#14740=CARTESIAN_POINT('Origin',(-1.22464679914735E-16,0.,1.));
#14741=CARTESIAN_POINT('',(-1.023815,-0.246528389340863,1.25381176266905E-16));
#14742=CARTESIAN_POINT('Origin',(0.,-0.246528389340863,0.));
#14743=CARTESIAN_POINT('Origin',(0.,-0.246528389340863,0.));
#14744=CARTESIAN_POINT('Origin',(0.,0.,0.));
#14745=CARTESIAN_POINT('',(-1.023815,-0.45,-1.25381176266905E-16));
#14746=CARTESIAN_POINT('Origin',(0.,-0.45,0.));
#14747=CARTESIAN_POINT('',(-1.023815,0.,-1.25381176266905E-16));
#14748=CARTESIAN_POINT('Origin',(1.44,0.45,0.));
#14749=CARTESIAN_POINT('',(-1.44,0.45,-1.76349139077219E-16));
#14750=CARTESIAN_POINT('Origin',(0.,0.45,0.));
#14751=CARTESIAN_POINT('',(-1.023815,0.45,-1.25381176266905E-16));
#14752=CARTESIAN_POINT('Origin',(0.,0.45,0.));
#14753=CARTESIAN_POINT('Origin',(0.,0.42,0.));
#14754=CARTESIAN_POINT('',(-1.5,0.39,-1.83697019872103E-16));
#14755=CARTESIAN_POINT('Origin',(0.,0.39,0.));
#14756=CARTESIAN_POINT('',(-1.47,0.42,-1.80023079474661E-16));
#14757=CARTESIAN_POINT('Origin',(0.,0.,0.));
#14758=CARTESIAN_POINT('',(-1.5,-0.39,-1.83697019872103E-16));
#14759=CARTESIAN_POINT('Origin',(0.,-0.39,0.));
#14760=CARTESIAN_POINT('',(-1.5,0.,-1.83697019872103E-16));
#14761=CARTESIAN_POINT('Origin',(0.,-0.42,0.));
#14762=CARTESIAN_POINT('',(-1.44,-0.45,-1.76349139077219E-16));
#14763=CARTESIAN_POINT('Origin',(0.,-0.45,0.));
#14764=CARTESIAN_POINT('',(-1.47,-0.42,-1.80023079474661E-16));
#14765=CARTESIAN_POINT('Origin',(1.023815,-0.45,0.));
#14766=CARTESIAN_POINT('Origin',(0.,0.,0.));
#14767=CARTESIAN_POINT('',(-1.023815,0.,-1.25381176266905E-16));
#14768=CARTESIAN_POINT('',(0.,0.,0.));
#14769=CARTESIAN_POINT('Origin',(1.,0.,0.));
#14770=CARTESIAN_POINT('',(1.,-1.78583896120461E-33,0.23815));
#14771=CARTESIAN_POINT('',(1.,-1.78583896120461E-33,-0.23815));
#14772=CARTESIAN_POINT('Origin',(1.,0.,0.));
#14773=CARTESIAN_POINT('Origin',(0.707106781186548,0.,-0.707106781186547));
#14774=CARTESIAN_POINT('',(0.875504261126124,-1.78583896120461E-33,-0.538709301246971));
#14775=CARTESIAN_POINT('',(0.538709301246971,-1.78583896120461E-33,-0.875504261126124));
#14776=CARTESIAN_POINT('Origin',(0.707106781186548,0.,-0.707106781186547));
#14777=CARTESIAN_POINT('Origin',(6.12323399573677E-17,0.,-1.));
#14778=CARTESIAN_POINT('',(0.23815,-1.78583896120461E-33,-1.));
#14779=CARTESIAN_POINT('',(-0.23815,-1.78583896120461E-33,-1.));
#14780=CARTESIAN_POINT('Origin',(6.12323399573677E-17,0.,-1.));
#14781=CARTESIAN_POINT('Origin',(-0.707106781186547,0.,-0.707106781186548));
#14782=CARTESIAN_POINT('',(-0.538709301246971,-1.78583896120461E-33,-0.875504261126124));
#14783=CARTESIAN_POINT('',(-0.875504261126124,-1.78583896120461E-33,-0.538709301246971));
#14784=CARTESIAN_POINT('Origin',(-0.707106781186547,0.,-0.707106781186548));
#14785=CARTESIAN_POINT('Origin',(-1.,0.,-1.22464679914735E-16));
#14786=CARTESIAN_POINT('',(-1.,-1.78583896120461E-33,-0.23815));
#14787=CARTESIAN_POINT('',(-1.,-1.78583896120461E-33,0.23815));
#14788=CARTESIAN_POINT('Origin',(-1.,0.,-1.22464679914735E-16));
#14789=CARTESIAN_POINT('Origin',(-0.707106781186548,0.,0.707106781186547));
#14790=CARTESIAN_POINT('',(-0.875504261126124,-7.94881478324376E-33,0.538709301246971));
#14791=CARTESIAN_POINT('',(-0.538709301246971,4.37713686083455E-33,0.875504261126124));
#14792=CARTESIAN_POINT('Origin',(-0.707106781186548,0.,0.707106781186547));
#14793=CARTESIAN_POINT('Origin',(-1.83697019872103E-16,0.,1.));
#14794=CARTESIAN_POINT('',(-0.23815,-1.78583896120461E-33,1.));
#14795=CARTESIAN_POINT('',(0.23815,-1.78583896120461E-33,1.));
#14796=CARTESIAN_POINT('Origin',(-1.83697019872103E-16,0.,1.));
#14797=CARTESIAN_POINT('Origin',(0.707106781186547,0.,0.707106781186548));
#14798=CARTESIAN_POINT('',(0.538709301246971,-4.86732687222419E-33,0.875504261126124));
#14799=CARTESIAN_POINT('',(0.875504261126124,1.29564894981497E-33,0.538709301246971));
#14800=CARTESIAN_POINT('Origin',(0.707106781186547,0.,0.707106781186548));
#14801=CARTESIAN_POINT('',(0.,0.,0.));
#14802=CARTESIAN_POINT('Origin',(0.707106781186547,0.,0.707106781186548));
#14803=CARTESIAN_POINT('',(0.504455939115715,-0.04763,0.841298510752802));
#14804=CARTESIAN_POINT('',(0.841298510752802,-0.04763,0.504455939115715));
#14805=CARTESIAN_POINT('Ctrl Pts',(0.504455939115715,-0.04763,0.841298510752802));
#14806=CARTESIAN_POINT('Ctrl Pts',(0.508899795931835,-0.0740444353928835,
0.838633903678357));
#14807=CARTESIAN_POINT('Ctrl Pts',(0.517157748491652,-0.0999305678883309,
0.833661031856294));
#14808=CARTESIAN_POINT('Ctrl Pts',(0.537715343527944,-0.142345102874864,
0.820511285096538));
#14809=CARTESIAN_POINT('Ctrl Pts',(0.548874290046456,-0.159766064500479,
0.813159949759));
#14810=CARTESIAN_POINT('Ctrl Pts',(0.573915184558107,-0.190326085855194,
0.795684265985089));
#14811=CARTESIAN_POINT('Ctrl Pts',(0.587792702767295,-0.203463743702801,
0.78555112003688));
#14812=CARTESIAN_POINT('Ctrl Pts',(0.615966552324775,-0.224161999508995,
0.763642258217233));
#14813=CARTESIAN_POINT('Ctrl Pts',(0.631684198665438,-0.232861760990032,
0.750785745543687));
#14814=CARTESIAN_POINT('Ctrl Pts',(0.663382628119203,-0.244251601209411,
0.722929908501543));
#14815=CARTESIAN_POINT('Ctrl Pts',(0.679352081686668,-0.246942143572133,
0.707917883896095));
#14816=CARTESIAN_POINT('Ctrl Pts',(0.707917883896095,-0.246942143572133,
0.679352081686668));
#14817=CARTESIAN_POINT('Ctrl Pts',(0.722929908501543,-0.244251601209411,
0.663382628119203));
#14818=CARTESIAN_POINT('Ctrl Pts',(0.750785745543687,-0.232861760990032,
0.631684198665439));
#14819=CARTESIAN_POINT('Ctrl Pts',(0.763642258217232,-0.224161999508995,
0.615966552324775));
#14820=CARTESIAN_POINT('Ctrl Pts',(0.78555112003688,-0.203463743702801,
0.587792702767295));
#14821=CARTESIAN_POINT('Ctrl Pts',(0.795684265985088,-0.190326085855194,
0.573915184558108));
#14822=CARTESIAN_POINT('Ctrl Pts',(0.813159949759,-0.15976606450048,0.548874290046456));
#14823=CARTESIAN_POINT('Ctrl Pts',(0.820511285096538,-0.142345102874864,
0.537715343527944));
#14824=CARTESIAN_POINT('Ctrl Pts',(0.833661031856294,-0.099930567888331,
0.517157748491653));
#14825=CARTESIAN_POINT('Ctrl Pts',(0.838633903678357,-0.0740444353928835,
0.508899795931835));
#14826=CARTESIAN_POINT('Ctrl Pts',(0.841298510752801,-0.0476299999999999,
0.504455939115715));
#14827=CARTESIAN_POINT('',(0.528110872004958,-0.04763,0.871530771444223));
#14828=CARTESIAN_POINT('Origin',(0.707106781186547,-0.04763,0.707106781186548));
#14829=CARTESIAN_POINT('',(0.871530771444223,-0.04763,0.528110872004959));
#14830=CARTESIAN_POINT('Ctrl Pts',(0.871530771444223,-0.0476300000000001,
0.528110872004958));
#14831=CARTESIAN_POINT('Ctrl Pts',(0.87014664509073,-0.0609922781173483,
0.530395067942936));
#14832=CARTESIAN_POINT('Ctrl Pts',(0.868149331745851,-0.0742967091364493,
0.533674141594226));
#14833=CARTESIAN_POINT('Ctrl Pts',(0.85981294420286,-0.115492077056649,
0.54708917182331));
#14834=CARTESIAN_POINT('Ctrl Pts',(0.850993704737257,-0.141695629206859,
0.560922177770136));
#14835=CARTESIAN_POINT('Ctrl Pts',(0.830754510485543,-0.181890537957859,
0.590422647829571));
#14836=CARTESIAN_POINT('Ctrl Pts',(0.816896541396381,-0.201072148666545,
0.609616703125488));
#14837=CARTESIAN_POINT('Ctrl Pts',(0.792310597819928,-0.223955109275652,
0.641117951819998));
#14838=CARTESIAN_POINT('Ctrl Pts',(0.779109323683612,-0.232742381310829,
0.657208095763053));
#14839=CARTESIAN_POINT('Ctrl Pts',(0.750552691816206,-0.244234834628584,
0.68964083160521));
#14840=CARTESIAN_POINT('Ctrl Pts',(0.735185187071673,-0.246942143572133,
0.705971972091755));
#14841=CARTESIAN_POINT('Ctrl Pts',(0.705971972091754,-0.246942143572133,
0.735185187071673));
#14842=CARTESIAN_POINT('Ctrl Pts',(0.689640831605209,-0.244234834628584,
0.750552691816206));
#14843=CARTESIAN_POINT('Ctrl Pts',(0.657208095763052,-0.232742381310829,
0.779109323683612));
#14844=CARTESIAN_POINT('Ctrl Pts',(0.641117951819998,-0.223955109275652,
0.792310597819928));
#14845=CARTESIAN_POINT('Ctrl Pts',(0.609616703125487,-0.201072148666545,
0.816896541396382));
#14846=CARTESIAN_POINT('Ctrl Pts',(0.590422647829571,-0.181890537957858,
0.830754510485544));
#14847=CARTESIAN_POINT('Ctrl Pts',(0.560922177770135,-0.141695629206858,
0.850993704737257));
#14848=CARTESIAN_POINT('Ctrl Pts',(0.547089171823309,-0.115492077056649,
0.859812944202861));
#14849=CARTESIAN_POINT('Ctrl Pts',(0.533674141594226,-0.0742967091364491,
0.868149331745852));
#14850=CARTESIAN_POINT('Ctrl Pts',(0.530395067942936,-0.0609922781173483,
0.870146645090731));
#14851=CARTESIAN_POINT('Ctrl Pts',(0.528110872004958,-0.0476300000000001,
0.871530771444223));
#14852=CARTESIAN_POINT('Origin',(0.707106781186547,-0.04763,0.707106781186548));
#14853=CARTESIAN_POINT('Origin',(0.,-0.166705,0.));
#14854=CARTESIAN_POINT('',(0.242834539687906,-0.04763,0.989696097314));
#14855=CARTESIAN_POINT('Origin',(0.,-0.04763,0.));
#14856=CARTESIAN_POINT('',(-0.242834539687907,-0.04763,0.989696097314));
#14857=CARTESIAN_POINT('Ctrl Pts',(0.242834539687906,-0.04763,0.989696097314));
#14858=CARTESIAN_POINT('Ctrl Pts',(0.24024064412003,-0.0609922781173483,
0.990332542620729));
#14859=CARTESIAN_POINT('Ctrl Pts',(0.236509675094874,-0.0742967091364492,
0.991238884025248));
#14860=CARTESIAN_POINT('Ctrl Pts',(0.221129100087819,-0.115492077056649,
0.994830026707808));
#14861=CARTESIAN_POINT('Ctrl Pts',(0.205111543747588,-0.141695629206859,
0.998375294985966));
#14862=CARTESIAN_POINT('Ctrl Pts',(0.169940289819232,-0.181890537957859,
1.00492400591205));
#14863=CARTESIAN_POINT('Ctrl Pts',(0.1465689792446,-0.201072148666545,1.00869718865384));
#14864=CARTESIAN_POINT('Ctrl Pts',(0.106909345252087,-0.223955109275652,
1.01358704779679));
#14865=CARTESIAN_POINT('Ctrl Pts',(0.0861971848975941,-0.232742381310829,
1.0156297872271));
#14866=CARTESIAN_POINT('Ctrl Pts',(0.0430711894098822,-0.244234834628584,
1.01837060663223));
#14867=CARTESIAN_POINT('Ctrl Pts',(0.0206568624125605,-0.246942143572133,
1.019052));
#14868=CARTESIAN_POINT('Ctrl Pts',(-0.0206568624125608,-0.246942143572133,
1.019052));
#14869=CARTESIAN_POINT('Ctrl Pts',(-0.0430711894098825,-0.244234834628584,
1.01837060663223));
#14870=CARTESIAN_POINT('Ctrl Pts',(-0.0861971848975943,-0.232742381310829,
1.0156297872271));
#14871=CARTESIAN_POINT('Ctrl Pts',(-0.106909345252088,-0.223955109275652,
1.01358704779679));
#14872=CARTESIAN_POINT('Ctrl Pts',(-0.1465689792446,-0.201072148666545,
1.00869718865384));
#14873=CARTESIAN_POINT('Ctrl Pts',(-0.169940289819232,-0.181890537957859,
1.00492400591205));
#14874=CARTESIAN_POINT('Ctrl Pts',(-0.205111543747588,-0.141695629206859,
0.998375294985966));
#14875=CARTESIAN_POINT('Ctrl Pts',(-0.221129100087819,-0.115492077056649,
0.994830026707808));
#14876=CARTESIAN_POINT('Ctrl Pts',(-0.236509675094875,-0.0742967091364493,
0.991238884025248));
#14877=CARTESIAN_POINT('Ctrl Pts',(-0.24024064412003,-0.0609922781173483,
0.990332542620729));
#14878=CARTESIAN_POINT('Ctrl Pts',(-0.242834539687907,-0.04763,0.989696097314));
#14879=CARTESIAN_POINT('',(-0.528110872004959,-0.04763,0.871530771444223));
#14880=CARTESIAN_POINT('Origin',(0.,-0.04763,0.));
#14881=CARTESIAN_POINT('',(-0.871530771444223,-0.04763,0.528110872004958));
#14882=CARTESIAN_POINT('Ctrl Pts',(-0.528110872004958,-0.0476300000000001,
0.871530771444223));
#14883=CARTESIAN_POINT('Ctrl Pts',(-0.530395067942936,-0.0609922781173484,
0.87014664509073));
#14884=CARTESIAN_POINT('Ctrl Pts',(-0.533674141594226,-0.0742967091364493,
0.868149331745851));
#14885=CARTESIAN_POINT('Ctrl Pts',(-0.54708917182331,-0.115492077056649,
0.85981294420286));
#14886=CARTESIAN_POINT('Ctrl Pts',(-0.560922177770136,-0.141695629206859,
0.850993704737257));
#14887=CARTESIAN_POINT('Ctrl Pts',(-0.590422647829571,-0.181890537957859,
0.830754510485543));
#14888=CARTESIAN_POINT('Ctrl Pts',(-0.609616703125488,-0.201072148666545,
0.816896541396381));
#14889=CARTESIAN_POINT('Ctrl Pts',(-0.641117951819998,-0.223955109275652,
0.792310597819928));
#14890=CARTESIAN_POINT('Ctrl Pts',(-0.657208095763053,-0.232742381310829,
0.779109323683611));
#14891=CARTESIAN_POINT('Ctrl Pts',(-0.68964083160521,-0.244234834628584,
0.750552691816205));
#14892=CARTESIAN_POINT('Ctrl Pts',(-0.705971972091755,-0.246942143572133,
0.735185187071673));
#14893=CARTESIAN_POINT('Ctrl Pts',(-0.735185187071673,-0.246942143572133,
0.705971972091754));
#14894=CARTESIAN_POINT('Ctrl Pts',(-0.750552691816206,-0.244234834628584,
0.689640831605209));
#14895=CARTESIAN_POINT('Ctrl Pts',(-0.779109323683612,-0.232742381310829,
0.657208095763052));
#14896=CARTESIAN_POINT('Ctrl Pts',(-0.792310597819928,-0.223955109275652,
0.641117951819998));
#14897=CARTESIAN_POINT('Ctrl Pts',(-0.816896541396382,-0.201072148666545,
0.609616703125487));
#14898=CARTESIAN_POINT('Ctrl Pts',(-0.830754510485544,-0.181890537957858,
0.590422647829571));
#14899=CARTESIAN_POINT('Ctrl Pts',(-0.850993704737257,-0.141695629206858,
0.560922177770135));
#14900=CARTESIAN_POINT('Ctrl Pts',(-0.859812944202861,-0.115492077056649,
0.547089171823309));
#14901=CARTESIAN_POINT('Ctrl Pts',(-0.868149331745852,-0.0742967091364491,
0.533674141594226));
#14902=CARTESIAN_POINT('Ctrl Pts',(-0.870146645090731,-0.0609922781173483,
0.530395067942936));
#14903=CARTESIAN_POINT('Ctrl Pts',(-0.871530771444223,-0.04763,0.528110872004958));
#14904=CARTESIAN_POINT('',(-0.989696097314,-0.04763,0.242834539687906));
#14905=CARTESIAN_POINT('Origin',(0.,-0.04763,0.));
#14906=CARTESIAN_POINT('',(-1.019052,-0.246942143572133,1.248489836334E-16));
#14907=CARTESIAN_POINT('Ctrl Pts',(-0.989696097314,-0.04763,0.242834539687906));
#14908=CARTESIAN_POINT('Ctrl Pts',(-0.990332542620729,-0.0609922781173483,
0.24024064412003));
#14909=CARTESIAN_POINT('Ctrl Pts',(-0.991238884025248,-0.0742967091364492,
0.236509675094874));
#14910=CARTESIAN_POINT('Ctrl Pts',(-0.994830026707808,-0.115492077056649,
0.221129100087819));
#14911=CARTESIAN_POINT('Ctrl Pts',(-0.998375294985966,-0.141695629206859,
0.205111543747588));
#14912=CARTESIAN_POINT('Ctrl Pts',(-1.00492400591205,-0.181890537957859,
0.169940289819232));
#14913=CARTESIAN_POINT('Ctrl Pts',(-1.00869718865384,-0.201072148666545,
0.1465689792446));
#14914=CARTESIAN_POINT('Ctrl Pts',(-1.01358704779679,-0.223955109275652,
0.106909345252088));
#14915=CARTESIAN_POINT('Ctrl Pts',(-1.0156297872271,-0.232742381310829,
0.0861971848975944));
#14916=CARTESIAN_POINT('Ctrl Pts',(-1.01837060663223,-0.244234834628584,
0.0430711894098825));
#14917=CARTESIAN_POINT('Ctrl Pts',(-1.019052,-0.246942143572133,0.0206568624125608));
#14918=CARTESIAN_POINT('Ctrl Pts',(-1.019052,-0.246942143572133,1.2490009027033E-16));
#14919=CARTESIAN_POINT('',(-1.019052,-0.28578,1.24797876996471E-16));
#14920=CARTESIAN_POINT('',(-1.019052,-0.166705,1.24797876996471E-16));
#14921=CARTESIAN_POINT('Origin',(0.,-0.28578,0.));
#14922=CARTESIAN_POINT('',(-0.989696097314,-0.04763,-0.242834539687906));
#14923=CARTESIAN_POINT('Ctrl Pts',(-1.019052,-0.246942143572133,1.2490009027033E-16));
#14924=CARTESIAN_POINT('Ctrl Pts',(-1.019052,-0.246942143572133,-0.0206568624125605));
#14925=CARTESIAN_POINT('Ctrl Pts',(-1.01837060663223,-0.244234834628584,
-0.0430711894098822));
#14926=CARTESIAN_POINT('Ctrl Pts',(-1.0156297872271,-0.232742381310829,
-0.0861971848975941));
#14927=CARTESIAN_POINT('Ctrl Pts',(-1.01358704779679,-0.223955109275652,
-0.106909345252087));
#14928=CARTESIAN_POINT('Ctrl Pts',(-1.00869718865384,-0.201072148666546,
-0.1465689792446));
#14929=CARTESIAN_POINT('Ctrl Pts',(-1.00492400591205,-0.181890537957859,
-0.169940289819232));
#14930=CARTESIAN_POINT('Ctrl Pts',(-0.998375294985966,-0.141695629206859,
-0.205111543747588));
#14931=CARTESIAN_POINT('Ctrl Pts',(-0.994830026707808,-0.11549207705665,
-0.221129100087819));
#14932=CARTESIAN_POINT('Ctrl Pts',(-0.991238884025248,-0.0742967091364495,
-0.236509675094874));
#14933=CARTESIAN_POINT('Ctrl Pts',(-0.990332542620729,-0.0609922781173484,
-0.24024064412003));
#14934=CARTESIAN_POINT('Ctrl Pts',(-0.989696097314,-0.0476300000000001,
-0.242834539687907));
#14935=CARTESIAN_POINT('',(-0.871530771444223,-0.04763,-0.528110872004958));
#14936=CARTESIAN_POINT('Origin',(0.,-0.04763,0.));
#14937=CARTESIAN_POINT('',(-0.528110872004958,-0.04763,-0.871530771444223));
#14938=CARTESIAN_POINT('Ctrl Pts',(-0.871530771444223,-0.0476300000000001,
-0.528110872004958));
#14939=CARTESIAN_POINT('Ctrl Pts',(-0.87014664509073,-0.0609922781173484,
-0.530395067942936));
#14940=CARTESIAN_POINT('Ctrl Pts',(-0.868149331745851,-0.0742967091364494,
-0.533674141594226));
#14941=CARTESIAN_POINT('Ctrl Pts',(-0.85981294420286,-0.115492077056649,
-0.54708917182331));
#14942=CARTESIAN_POINT('Ctrl Pts',(-0.850993704737257,-0.141695629206859,
-0.560922177770136));
#14943=CARTESIAN_POINT('Ctrl Pts',(-0.830754510485543,-0.181890537957859,
-0.590422647829571));
#14944=CARTESIAN_POINT('Ctrl Pts',(-0.816896541396381,-0.201072148666546,
-0.609616703125488));
#14945=CARTESIAN_POINT('Ctrl Pts',(-0.792310597819928,-0.223955109275652,
-0.641117951819999));
#14946=CARTESIAN_POINT('Ctrl Pts',(-0.779109323683611,-0.232742381310829,
-0.657208095763053));
#14947=CARTESIAN_POINT('Ctrl Pts',(-0.750552691816205,-0.244234834628584,
-0.68964083160521));
#14948=CARTESIAN_POINT('Ctrl Pts',(-0.735185187071673,-0.246942143572133,
-0.705971972091755));
#14949=CARTESIAN_POINT('Ctrl Pts',(-0.705971972091754,-0.246942143572133,
-0.735185187071673));
#14950=CARTESIAN_POINT('Ctrl Pts',(-0.68964083160521,-0.244234834628584,
-0.750552691816206));
#14951=CARTESIAN_POINT('Ctrl Pts',(-0.657208095763052,-0.232742381310829,
-0.779109323683612));
#14952=CARTESIAN_POINT('Ctrl Pts',(-0.641117951819998,-0.223955109275652,
-0.792310597819928));
#14953=CARTESIAN_POINT('Ctrl Pts',(-0.609616703125488,-0.201072148666545,
-0.816896541396381));
#14954=CARTESIAN_POINT('Ctrl Pts',(-0.590422647829571,-0.181890537957859,
-0.830754510485543));
#14955=CARTESIAN_POINT('Ctrl Pts',(-0.560922177770136,-0.141695629206859,
-0.850993704737257));
#14956=CARTESIAN_POINT('Ctrl Pts',(-0.54708917182331,-0.115492077056649,
-0.85981294420286));
#14957=CARTESIAN_POINT('Ctrl Pts',(-0.533674141594226,-0.0742967091364494,
-0.868149331745852));
#14958=CARTESIAN_POINT('Ctrl Pts',(-0.530395067942936,-0.0609922781173484,
-0.870146645090731));
#14959=CARTESIAN_POINT('Ctrl Pts',(-0.528110872004958,-0.0476300000000001,
-0.871530771444223));
#14960=CARTESIAN_POINT('',(-0.242834539687906,-0.04763,-0.989696097314));
#14961=CARTESIAN_POINT('Origin',(0.,-0.04763,0.));
#14962=CARTESIAN_POINT('',(0.242834539687906,-0.04763,-0.989696097314));
#14963=CARTESIAN_POINT('Ctrl Pts',(-0.242834539687907,-0.04763,-0.989696097314));
#14964=CARTESIAN_POINT('Ctrl Pts',(-0.24024064412003,-0.0609922781173483,
-0.990332542620729));
#14965=CARTESIAN_POINT('Ctrl Pts',(-0.236509675094874,-0.0742967091364493,
-0.991238884025248));
#14966=CARTESIAN_POINT('Ctrl Pts',(-0.221129100087819,-0.115492077056649,
-0.994830026707808));
#14967=CARTESIAN_POINT('Ctrl Pts',(-0.205111543747588,-0.141695629206859,
-0.998375294985966));
#14968=CARTESIAN_POINT('Ctrl Pts',(-0.169940289819232,-0.181890537957859,
-1.00492400591205));
#14969=CARTESIAN_POINT('Ctrl Pts',(-0.1465689792446,-0.201072148666545,
-1.00869718865384));
#14970=CARTESIAN_POINT('Ctrl Pts',(-0.106909345252087,-0.223955109275652,
-1.01358704779679));
#14971=CARTESIAN_POINT('Ctrl Pts',(-0.0861971848975942,-0.232742381310829,
-1.0156297872271));
#14972=CARTESIAN_POINT('Ctrl Pts',(-0.0430711894098823,-0.244234834628584,
-1.01837060663223));
#14973=CARTESIAN_POINT('Ctrl Pts',(-0.0206568624125606,-0.246942143572133,
-1.019052));
#14974=CARTESIAN_POINT('Ctrl Pts',(0.0206568624125607,-0.246942143572133,
-1.019052));
#14975=CARTESIAN_POINT('Ctrl Pts',(0.0430711894098824,-0.244234834628584,
-1.01837060663223));
#14976=CARTESIAN_POINT('Ctrl Pts',(0.0861971848975943,-0.232742381310829,
-1.0156297872271));
#14977=CARTESIAN_POINT('Ctrl Pts',(0.106909345252088,-0.223955109275652,
-1.01358704779679));
#14978=CARTESIAN_POINT('Ctrl Pts',(0.1465689792446,-0.201072148666545,-1.00869718865384));
#14979=CARTESIAN_POINT('Ctrl Pts',(0.169940289819232,-0.181890537957859,
-1.00492400591205));
#14980=CARTESIAN_POINT('Ctrl Pts',(0.205111543747588,-0.141695629206859,
-0.998375294985966));
#14981=CARTESIAN_POINT('Ctrl Pts',(0.221129100087819,-0.115492077056649,
-0.994830026707808));
#14982=CARTESIAN_POINT('Ctrl Pts',(0.236509675094874,-0.0742967091364493,
-0.991238884025248));
#14983=CARTESIAN_POINT('Ctrl Pts',(0.24024064412003,-0.0609922781173484,
-0.990332542620729));
#14984=CARTESIAN_POINT('Ctrl Pts',(0.242834539687907,-0.04763,-0.989696097314));
#14985=CARTESIAN_POINT('',(0.528110872004958,-0.04763,-0.871530771444223));
#14986=CARTESIAN_POINT('Origin',(0.,-0.04763,0.));
#14987=CARTESIAN_POINT('',(0.871530771444223,-0.04763,-0.528110872004958));
#14988=CARTESIAN_POINT('Ctrl Pts',(0.528110872004958,-0.0476300000000001,
-0.871530771444223));
#14989=CARTESIAN_POINT('Ctrl Pts',(0.530395067942936,-0.0609922781173484,
-0.870146645090731));
#14990=CARTESIAN_POINT('Ctrl Pts',(0.533674141594226,-0.0742967091364493,
-0.868149331745851));
#14991=CARTESIAN_POINT('Ctrl Pts',(0.54708917182331,-0.115492077056649,
-0.85981294420286));
#14992=CARTESIAN_POINT('Ctrl Pts',(0.560922177770136,-0.141695629206859,
-0.850993704737257));
#14993=CARTESIAN_POINT('Ctrl Pts',(0.590422647829571,-0.181890537957859,
-0.830754510485543));
#14994=CARTESIAN_POINT('Ctrl Pts',(0.609616703125488,-0.201072148666545,
-0.816896541396381));
#14995=CARTESIAN_POINT('Ctrl Pts',(0.641117951819998,-0.223955109275652,
-0.792310597819928));
#14996=CARTESIAN_POINT('Ctrl Pts',(0.657208095763053,-0.232742381310829,
-0.779109323683612));
#14997=CARTESIAN_POINT('Ctrl Pts',(0.68964083160521,-0.244234834628584,
-0.750552691816206));
#14998=CARTESIAN_POINT('Ctrl Pts',(0.705971972091755,-0.246942143572133,
-0.735185187071673));
#14999=CARTESIAN_POINT('Ctrl Pts',(0.735185187071673,-0.246942143572133,
-0.705971972091754));
#15000=CARTESIAN_POINT('Ctrl Pts',(0.750552691816206,-0.244234834628584,
-0.68964083160521));
#15001=CARTESIAN_POINT('Ctrl Pts',(0.779109323683612,-0.232742381310829,
-0.657208095763053));
#15002=CARTESIAN_POINT('Ctrl Pts',(0.792310597819928,-0.223955109275652,
-0.641117951819998));
#15003=CARTESIAN_POINT('Ctrl Pts',(0.816896541396381,-0.201072148666545,
-0.609616703125488));
#15004=CARTESIAN_POINT('Ctrl Pts',(0.830754510485543,-0.181890537957859,
-0.590422647829571));
#15005=CARTESIAN_POINT('Ctrl Pts',(0.850993704737257,-0.141695629206859,
-0.560922177770136));
#15006=CARTESIAN_POINT('Ctrl Pts',(0.85981294420286,-0.115492077056649,
-0.54708917182331));
#15007=CARTESIAN_POINT('Ctrl Pts',(0.868149331745851,-0.0742967091364493,
-0.533674141594226));
#15008=CARTESIAN_POINT('Ctrl Pts',(0.870146645090731,-0.0609922781173484,
-0.530395067942936));
#15009=CARTESIAN_POINT('Ctrl Pts',(0.871530771444223,-0.0476300000000001,
-0.528110872004958));
#15010=CARTESIAN_POINT('',(0.989696097314,-0.04763,-0.242834539687906));
#15011=CARTESIAN_POINT('Origin',(0.,-0.04763,0.));
#15012=CARTESIAN_POINT('',(0.989696097314,-0.04763,0.242834539687906));
#15013=CARTESIAN_POINT('Ctrl Pts',(0.989696097314,-0.04763,-0.242834539687907));
#15014=CARTESIAN_POINT('Ctrl Pts',(0.990332542620729,-0.0609922781173483,
-0.24024064412003));
#15015=CARTESIAN_POINT('Ctrl Pts',(0.991238884025248,-0.0742967091364493,
-0.236509675094874));
#15016=CARTESIAN_POINT('Ctrl Pts',(0.994830026707808,-0.115492077056649,
-0.221129100087819));
#15017=CARTESIAN_POINT('Ctrl Pts',(0.998375294985966,-0.141695629206859,
-0.205111543747588));
#15018=CARTESIAN_POINT('Ctrl Pts',(1.00492400591205,-0.181890537957859,
-0.169940289819232));
#15019=CARTESIAN_POINT('Ctrl Pts',(1.00869718865384,-0.201072148666545,
-0.1465689792446));
#15020=CARTESIAN_POINT('Ctrl Pts',(1.01358704779679,-0.223955109275652,
-0.106909345252087));
#15021=CARTESIAN_POINT('Ctrl Pts',(1.0156297872271,-0.232742381310829,-0.0861971848975942));
#15022=CARTESIAN_POINT('Ctrl Pts',(1.01837060663223,-0.244234834628584,
-0.0430711894098823));
#15023=CARTESIAN_POINT('Ctrl Pts',(1.019052,-0.246942143572133,-0.0206568624125607));
#15024=CARTESIAN_POINT('Ctrl Pts',(1.019052,-0.246942143572133,0.0206568624125607));
#15025=CARTESIAN_POINT('Ctrl Pts',(1.01837060663223,-0.244234834628584,
0.0430711894098823));
#15026=CARTESIAN_POINT('Ctrl Pts',(1.0156297872271,-0.232742381310829,0.0861971848975942));
#15027=CARTESIAN_POINT('Ctrl Pts',(1.01358704779679,-0.223955109275652,
0.106909345252087));
#15028=CARTESIAN_POINT('Ctrl Pts',(1.00869718865384,-0.201072148666545,
0.1465689792446));
#15029=CARTESIAN_POINT('Ctrl Pts',(1.00492400591205,-0.181890537957859,
0.169940289819232));
#15030=CARTESIAN_POINT('Ctrl Pts',(0.998375294985966,-0.141695629206859,
0.205111543747588));
#15031=CARTESIAN_POINT('Ctrl Pts',(0.994830026707808,-0.115492077056649,
0.221129100087819));
#15032=CARTESIAN_POINT('Ctrl Pts',(0.991238884025248,-0.0742967091364492,
0.236509675094874));
#15033=CARTESIAN_POINT('Ctrl Pts',(0.990332542620729,-0.0609922781173483,
0.24024064412003));
#15034=CARTESIAN_POINT('Ctrl Pts',(0.989696097314,-0.04763,0.242834539687907));
#15035=CARTESIAN_POINT('Origin',(0.,-0.04763,0.));
#15036=CARTESIAN_POINT('Origin',(0.,-0.04763,0.));
#15037=CARTESIAN_POINT('',(0.238183666596899,-0.04763,0.951592097314));
#15038=CARTESIAN_POINT('Origin',(0.,-0.04763,0.));
#15039=CARTESIAN_POINT('Origin',(-1.94289029309402E-16,-0.04763,1.));
#15040=CARTESIAN_POINT('Origin',(-1.94289029309402E-16,0.,1.));
#15041=CARTESIAN_POINT('',(-0.2381836665969,-0.04763,0.951592097314));
#15042=CARTESIAN_POINT('Ctrl Pts',(-0.238183666596899,-0.0476299999999999,
0.951592097314));
#15043=CARTESIAN_POINT('Ctrl Pts',(-0.233157223576062,-0.0740444353928835,
0.952850216871763));
#15044=CARTESIAN_POINT('Ctrl Pts',(-0.223801617934946,-0.0999305678883309,
0.955173119738174));
#15045=CARTESIAN_POINT('Ctrl Pts',(-0.199966927975188,-0.142345102874864,
0.960411259488514));
#15046=CARTESIAN_POINT('Ctrl Pts',(-0.1868781821531,-0.159766064500479,
0.963103647174702));
#15047=CARTESIAN_POINT('Ctrl Pts',(-0.15681442133453,-0.190326085855194,
0.968453058988463));
#15048=CARTESIAN_POINT('Ctrl Pts',(-0.139836317888043,-0.203463743702801,
0.971100730005489));
#15049=CARTESIAN_POINT('Ctrl Pts',(-0.104422493053067,-0.224161999508995,
0.975530745318961));
#15050=CARTESIAN_POINT('Ctrl Pts',(-0.0842175114474176,-0.232861760990032,
0.977553872336861));
#15051=CARTESIAN_POINT('Ctrl Pts',(-0.0421062857595701,-0.244251601209411,
0.980270995488453));
#15052=CARTESIAN_POINT('Ctrl Pts',(-0.0201990724523197,-0.246942143572133,
0.980948));
#15053=CARTESIAN_POINT('Ctrl Pts',(0.020199072452319,-0.246942143572133,
0.980948));
#15054=CARTESIAN_POINT('Ctrl Pts',(0.0421062857595694,-0.244251601209411,
0.980270995488454));
#15055=CARTESIAN_POINT('Ctrl Pts',(0.0842175114474169,-0.232861760990032,
0.977553872336861));
#15056=CARTESIAN_POINT('Ctrl Pts',(0.104422493053067,-0.224161999508995,
0.975530745318961));
#15057=CARTESIAN_POINT('Ctrl Pts',(0.139836317888042,-0.203463743702801,
0.971100730005489));
#15058=CARTESIAN_POINT('Ctrl Pts',(0.15681442133453,-0.190326085855194,
0.968453058988463));
#15059=CARTESIAN_POINT('Ctrl Pts',(0.1868781821531,-0.15976606450048,0.963103647174702));
#15060=CARTESIAN_POINT('Ctrl Pts',(0.199966927975188,-0.142345102874864,
0.960411259488514));
#15061=CARTESIAN_POINT('Ctrl Pts',(0.223801617934945,-0.0999305678883309,
0.955173119738174));
#15062=CARTESIAN_POINT('Ctrl Pts',(0.233157223576061,-0.0740444353928835,
0.952850216871763));
#15063=CARTESIAN_POINT('Ctrl Pts',(0.238183666596899,-0.0476299999999999,
0.951592097314));
#15064=CARTESIAN_POINT('Origin',(-1.94289029309402E-16,-0.04763,1.));
#15065=CARTESIAN_POINT('Origin',(0.,-0.04763,0.));
#15066=CARTESIAN_POINT('',(-0.504455939115715,-0.04763,0.841298510752802));
#15067=CARTESIAN_POINT('Origin',(0.,-0.04763,0.));
#15068=CARTESIAN_POINT('Origin',(-0.707106781186548,-0.04763,0.707106781186547));
#15069=CARTESIAN_POINT('Origin',(-0.707106781186548,0.,0.707106781186547));
#15070=CARTESIAN_POINT('',(-0.841298510752802,-0.04763,0.504455939115715));
#15071=CARTESIAN_POINT('Ctrl Pts',(-0.841298510752802,-0.04763,0.504455939115715));
#15072=CARTESIAN_POINT('Ctrl Pts',(-0.838633903678357,-0.0740444353928835,
0.508899795931835));
#15073=CARTESIAN_POINT('Ctrl Pts',(-0.833661031856294,-0.0999305678883309,
0.517157748491652));
#15074=CARTESIAN_POINT('Ctrl Pts',(-0.820511285096538,-0.142345102874864,
0.537715343527944));
#15075=CARTESIAN_POINT('Ctrl Pts',(-0.813159949759,-0.159766064500479,0.548874290046456));
#15076=CARTESIAN_POINT('Ctrl Pts',(-0.795684265985089,-0.190326085855194,
0.573915184558107));
#15077=CARTESIAN_POINT('Ctrl Pts',(-0.78555112003688,-0.203463743702801,
0.587792702767295));
#15078=CARTESIAN_POINT('Ctrl Pts',(-0.763642258217233,-0.224161999508995,
0.615966552324775));
#15079=CARTESIAN_POINT('Ctrl Pts',(-0.750785745543687,-0.232861760990032,
0.631684198665438));
#15080=CARTESIAN_POINT('Ctrl Pts',(-0.722929908501543,-0.244251601209411,
0.663382628119203));
#15081=CARTESIAN_POINT('Ctrl Pts',(-0.707917883896095,-0.246942143572133,
0.679352081686668));
#15082=CARTESIAN_POINT('Ctrl Pts',(-0.679352081686668,-0.246942143572133,
0.707917883896095));
#15083=CARTESIAN_POINT('Ctrl Pts',(-0.663382628119203,-0.244251601209411,
0.722929908501544));
#15084=CARTESIAN_POINT('Ctrl Pts',(-0.631684198665438,-0.232861760990031,
0.750785745543687));
#15085=CARTESIAN_POINT('Ctrl Pts',(-0.615966552324775,-0.224161999508995,
0.763642258217233));
#15086=CARTESIAN_POINT('Ctrl Pts',(-0.587792702767295,-0.203463743702801,
0.78555112003688));
#15087=CARTESIAN_POINT('Ctrl Pts',(-0.573915184558107,-0.190326085855194,
0.795684265985088));
#15088=CARTESIAN_POINT('Ctrl Pts',(-0.548874290046456,-0.159766064500479,
0.813159949759));
#15089=CARTESIAN_POINT('Ctrl Pts',(-0.537715343527944,-0.142345102874864,
0.820511285096538));
#15090=CARTESIAN_POINT('Ctrl Pts',(-0.517157748491652,-0.0999305678883309,
0.833661031856294));
#15091=CARTESIAN_POINT('Ctrl Pts',(-0.508899795931835,-0.0740444353928835,
0.838633903678357));
#15092=CARTESIAN_POINT('Ctrl Pts',(-0.504455939115716,-0.04763,0.841298510752801));
#15093=CARTESIAN_POINT('Origin',(-0.707106781186548,-0.04763,0.707106781186547));
#15094=CARTESIAN_POINT('Origin',(0.,-0.04763,0.));
#15095=CARTESIAN_POINT('',(-0.951592097314,-0.04763,0.238183666596899));
#15096=CARTESIAN_POINT('Origin',(0.,-0.04763,0.));
#15097=CARTESIAN_POINT('Origin',(-1.,-0.04763,-1.11022302462516E-16));
#15098=CARTESIAN_POINT('Origin',(-1.,0.,-1.11022302462516E-16));
#15099=CARTESIAN_POINT('',(-0.951592097314,-0.04763,-0.2381836665969));
#15100=CARTESIAN_POINT('',(-0.980948,-0.246942143572133,1.08514323328844E-18));
#15101=CARTESIAN_POINT('Ctrl Pts',(-0.951592097314,-0.04763,-0.238183666596899));
#15102=CARTESIAN_POINT('Ctrl Pts',(-0.952850216871763,-0.0740444353928835,
-0.233157223576062));
#15103=CARTESIAN_POINT('Ctrl Pts',(-0.955173119738174,-0.0999305678883309,
-0.223801617934946));
#15104=CARTESIAN_POINT('Ctrl Pts',(-0.960411259488514,-0.142345102874864,
-0.199966927975188));
#15105=CARTESIAN_POINT('Ctrl Pts',(-0.963103647174702,-0.159766064500479,
-0.1868781821531));
#15106=CARTESIAN_POINT('Ctrl Pts',(-0.968453058988463,-0.190326085855194,
-0.15681442133453));
#15107=CARTESIAN_POINT('Ctrl Pts',(-0.971100730005489,-0.203463743702801,
-0.139836317888043));
#15108=CARTESIAN_POINT('Ctrl Pts',(-0.975530745318961,-0.224161999508995,
-0.104422493053067));
#15109=CARTESIAN_POINT('Ctrl Pts',(-0.977553872336861,-0.232861760990032,
-0.0842175114474175));
#15110=CARTESIAN_POINT('Ctrl Pts',(-0.980270995488453,-0.244251601209411,
-0.0421062857595699));
#15111=CARTESIAN_POINT('Ctrl Pts',(-0.980948,-0.246942143572133,-0.0201990724523195));
#15112=CARTESIAN_POINT('Ctrl Pts',(-0.980948,-0.246942143572133,-1.17961196366423E-16));
#15113=CARTESIAN_POINT('Origin',(-1.,-0.04763,-1.11022302462516E-16));
#15114=CARTESIAN_POINT('Ctrl Pts',(-0.980948,-0.246942143572133,-1.17961196366423E-16));
#15115=CARTESIAN_POINT('Ctrl Pts',(-0.980948,-0.246942143572133,0.0201990724523192));
#15116=CARTESIAN_POINT('Ctrl Pts',(-0.980270995488453,-0.244251601209411,
0.0421062857595695));
#15117=CARTESIAN_POINT('Ctrl Pts',(-0.977553872336861,-0.232861760990032,
0.0842175114474169));
#15118=CARTESIAN_POINT('Ctrl Pts',(-0.975530745318961,-0.224161999508995,
0.104422493053066));
#15119=CARTESIAN_POINT('Ctrl Pts',(-0.971100730005489,-0.203463743702801,
0.139836317888042));
#15120=CARTESIAN_POINT('Ctrl Pts',(-0.968453058988463,-0.190326085855194,
0.15681442133453));
#15121=CARTESIAN_POINT('Ctrl Pts',(-0.963103647174702,-0.15976606450048,
0.1868781821531));
#15122=CARTESIAN_POINT('Ctrl Pts',(-0.960411259488514,-0.142345102874864,
0.199966927975188));
#15123=CARTESIAN_POINT('Ctrl Pts',(-0.955173119738174,-0.099930567888331,
0.223801617934945));
#15124=CARTESIAN_POINT('Ctrl Pts',(-0.952850216871763,-0.0740444353928835,
0.233157223576061));
#15125=CARTESIAN_POINT('Ctrl Pts',(-0.951592097314,-0.04763,0.238183666596899));
#15126=CARTESIAN_POINT('Origin',(0.,-0.04763,0.));
#15127=CARTESIAN_POINT('',(-0.841298510752802,-0.04763,-0.504455939115715));
#15128=CARTESIAN_POINT('Origin',(0.,-0.04763,0.));
#15129=CARTESIAN_POINT('Origin',(-0.707106781186547,-0.04763,-0.707106781186548));
#15130=CARTESIAN_POINT('Origin',(-0.707106781186547,0.,-0.707106781186548));
#15131=CARTESIAN_POINT('',(-0.504455939115715,-0.04763,-0.841298510752802));
#15132=CARTESIAN_POINT('Ctrl Pts',(-0.504455939115715,-0.04763,-0.841298510752802));
#15133=CARTESIAN_POINT('Ctrl Pts',(-0.508899795931835,-0.0740444353928835,
-0.838633903678357));
#15134=CARTESIAN_POINT('Ctrl Pts',(-0.517157748491652,-0.0999305678883309,
-0.833661031856294));
#15135=CARTESIAN_POINT('Ctrl Pts',(-0.537715343527944,-0.142345102874864,
-0.820511285096538));
#15136=CARTESIAN_POINT('Ctrl Pts',(-0.548874290046456,-0.159766064500479,
-0.813159949759));
#15137=CARTESIAN_POINT('Ctrl Pts',(-0.573915184558107,-0.190326085855194,
-0.795684265985089));
#15138=CARTESIAN_POINT('Ctrl Pts',(-0.587792702767295,-0.203463743702801,
-0.78555112003688));
#15139=CARTESIAN_POINT('Ctrl Pts',(-0.615966552324775,-0.224161999508995,
-0.763642258217233));
#15140=CARTESIAN_POINT('Ctrl Pts',(-0.631684198665438,-0.232861760990032,
-0.750785745543687));
#15141=CARTESIAN_POINT('Ctrl Pts',(-0.663382628119203,-0.244251601209411,
-0.722929908501543));
#15142=CARTESIAN_POINT('Ctrl Pts',(-0.679352081686668,-0.246942143572133,
-0.707917883896095));
#15143=CARTESIAN_POINT('Ctrl Pts',(-0.707917883896095,-0.246942143572133,
-0.679352081686668));
#15144=CARTESIAN_POINT('Ctrl Pts',(-0.722929908501543,-0.244251601209411,
-0.663382628119203));
#15145=CARTESIAN_POINT('Ctrl Pts',(-0.750785745543687,-0.232861760990032,
-0.631684198665439));
#15146=CARTESIAN_POINT('Ctrl Pts',(-0.763642258217232,-0.224161999508995,
-0.615966552324775));
#15147=CARTESIAN_POINT('Ctrl Pts',(-0.78555112003688,-0.203463743702801,
-0.587792702767295));
#15148=CARTESIAN_POINT('Ctrl Pts',(-0.795684265985088,-0.190326085855194,
-0.573915184558107));
#15149=CARTESIAN_POINT('Ctrl Pts',(-0.813159949759,-0.15976606450048,-0.548874290046456));
#15150=CARTESIAN_POINT('Ctrl Pts',(-0.820511285096538,-0.142345102874864,
-0.537715343527944));
#15151=CARTESIAN_POINT('Ctrl Pts',(-0.833661031856294,-0.0999305678883311,
-0.517157748491652));
#15152=CARTESIAN_POINT('Ctrl Pts',(-0.838633903678357,-0.0740444353928836,
-0.508899795931835));
#15153=CARTESIAN_POINT('Ctrl Pts',(-0.841298510752801,-0.04763,-0.504455939115715));
#15154=CARTESIAN_POINT('Origin',(-0.707106781186547,-0.04763,-0.707106781186548));
#15155=CARTESIAN_POINT('Origin',(0.,-0.04763,0.));
#15156=CARTESIAN_POINT('',(-0.238183666596899,-0.04763,-0.951592097314));
#15157=CARTESIAN_POINT('Origin',(0.,-0.04763,0.));
#15158=CARTESIAN_POINT('Origin',(5.55111512312578E-17,-0.04763,-1.));
#15159=CARTESIAN_POINT('Origin',(5.55111512312578E-17,0.,-1.));
#15160=CARTESIAN_POINT('',(0.238183666596899,-0.04763,-0.951592097314));
#15161=CARTESIAN_POINT('Ctrl Pts',(0.238183666596899,-0.04763,-0.951592097314));
#15162=CARTESIAN_POINT('Ctrl Pts',(0.233157223576062,-0.0740444353928835,
-0.952850216871763));
#15163=CARTESIAN_POINT('Ctrl Pts',(0.223801617934946,-0.099930567888331,
-0.955173119738174));
#15164=CARTESIAN_POINT('Ctrl Pts',(0.199966927975188,-0.142345102874864,
-0.960411259488514));
#15165=CARTESIAN_POINT('Ctrl Pts',(0.1868781821531,-0.15976606450048,-0.963103647174702));
#15166=CARTESIAN_POINT('Ctrl Pts',(0.15681442133453,-0.190326085855194,
-0.968453058988463));
#15167=CARTESIAN_POINT('Ctrl Pts',(0.139836317888042,-0.203463743702801,
-0.971100730005489));
#15168=CARTESIAN_POINT('Ctrl Pts',(0.104422493053067,-0.224161999508995,
-0.975530745318961));
#15169=CARTESIAN_POINT('Ctrl Pts',(0.0842175114474173,-0.232861760990032,
-0.977553872336861));
#15170=CARTESIAN_POINT('Ctrl Pts',(0.0421062857595698,-0.244251601209411,
-0.980270995488453));
#15171=CARTESIAN_POINT('Ctrl Pts',(0.0201990724523194,-0.246942143572133,
-0.980948));
#15172=CARTESIAN_POINT('Ctrl Pts',(-0.0201990724523193,-0.246942143572133,
-0.980948));
#15173=CARTESIAN_POINT('Ctrl Pts',(-0.0421062857595697,-0.244251601209411,
-0.980270995488453));
#15174=CARTESIAN_POINT('Ctrl Pts',(-0.0842175114474171,-0.232861760990032,
-0.977553872336861));
#15175=CARTESIAN_POINT('Ctrl Pts',(-0.104422493053067,-0.224161999508995,
-0.975530745318961));
#15176=CARTESIAN_POINT('Ctrl Pts',(-0.139836317888042,-0.203463743702801,
-0.971100730005489));
#15177=CARTESIAN_POINT('Ctrl Pts',(-0.15681442133453,-0.190326085855194,
-0.968453058988463));
#15178=CARTESIAN_POINT('Ctrl Pts',(-0.1868781821531,-0.15976606450048,-0.963103647174702));
#15179=CARTESIAN_POINT('Ctrl Pts',(-0.199966927975188,-0.142345102874864,
-0.960411259488514));
#15180=CARTESIAN_POINT('Ctrl Pts',(-0.223801617934945,-0.099930567888331,
-0.955173119738174));
#15181=CARTESIAN_POINT('Ctrl Pts',(-0.233157223576062,-0.0740444353928835,
-0.952850216871763));
#15182=CARTESIAN_POINT('Ctrl Pts',(-0.238183666596899,-0.0476299999999999,
-0.951592097314));
#15183=CARTESIAN_POINT('Origin',(5.55111512312578E-17,-0.04763,-1.));
#15184=CARTESIAN_POINT('Origin',(0.,-0.04763,0.));
#15185=CARTESIAN_POINT('',(0.504455939115715,-0.04763,-0.841298510752802));
#15186=CARTESIAN_POINT('Origin',(0.,-0.04763,0.));
#15187=CARTESIAN_POINT('Origin',(0.707106781186548,-0.04763,-0.707106781186547));
#15188=CARTESIAN_POINT('Origin',(0.707106781186548,0.,-0.707106781186547));
#15189=CARTESIAN_POINT('',(0.841298510752802,-0.04763,-0.504455939115715));
#15190=CARTESIAN_POINT('Ctrl Pts',(0.841298510752802,-0.04763,-0.504455939115715));
#15191=CARTESIAN_POINT('Ctrl Pts',(0.838633903678357,-0.0740444353928835,
-0.508899795931835));
#15192=CARTESIAN_POINT('Ctrl Pts',(0.833661031856294,-0.0999305678883309,
-0.517157748491652));
#15193=CARTESIAN_POINT('Ctrl Pts',(0.820511285096538,-0.142345102874864,
-0.537715343527944));
#15194=CARTESIAN_POINT('Ctrl Pts',(0.813159949759,-0.159766064500479,-0.548874290046456));
#15195=CARTESIAN_POINT('Ctrl Pts',(0.795684265985088,-0.190326085855194,
-0.573915184558107));
#15196=CARTESIAN_POINT('Ctrl Pts',(0.78555112003688,-0.203463743702801,
-0.587792702767295));
#15197=CARTESIAN_POINT('Ctrl Pts',(0.763642258217233,-0.224161999508995,
-0.615966552324775));
#15198=CARTESIAN_POINT('Ctrl Pts',(0.750785745543687,-0.232861760990032,
-0.631684198665438));
#15199=CARTESIAN_POINT('Ctrl Pts',(0.722929908501543,-0.244251601209411,
-0.663382628119203));
#15200=CARTESIAN_POINT('Ctrl Pts',(0.707917883896095,-0.246942143572133,
-0.679352081686668));
#15201=CARTESIAN_POINT('Ctrl Pts',(0.679352081686668,-0.246942143572133,
-0.707917883896095));
#15202=CARTESIAN_POINT('Ctrl Pts',(0.663382628119203,-0.244251601209411,
-0.722929908501543));
#15203=CARTESIAN_POINT('Ctrl Pts',(0.631684198665438,-0.232861760990032,
-0.750785745543687));
#15204=CARTESIAN_POINT('Ctrl Pts',(0.615966552324775,-0.224161999508995,
-0.763642258217232));
#15205=CARTESIAN_POINT('Ctrl Pts',(0.587792702767295,-0.203463743702801,
-0.78555112003688));
#15206=CARTESIAN_POINT('Ctrl Pts',(0.573915184558107,-0.190326085855194,
-0.795684265985088));
#15207=CARTESIAN_POINT('Ctrl Pts',(0.548874290046456,-0.159766064500479,
-0.813159949759));
#15208=CARTESIAN_POINT('Ctrl Pts',(0.537715343527944,-0.142345102874864,
-0.820511285096538));
#15209=CARTESIAN_POINT('Ctrl Pts',(0.517157748491652,-0.099930567888331,
-0.833661031856294));
#15210=CARTESIAN_POINT('Ctrl Pts',(0.508899795931835,-0.0740444353928835,
-0.838633903678357));
#15211=CARTESIAN_POINT('Ctrl Pts',(0.504455939115715,-0.04763,-0.841298510752801));
#15212=CARTESIAN_POINT('Origin',(0.707106781186548,-0.04763,-0.707106781186547));
#15213=CARTESIAN_POINT('Origin',(0.,-0.166705,0.));
#15214=CARTESIAN_POINT('',(-0.980948,-0.28578,1.20131482833E-16));
#15215=CARTESIAN_POINT('Origin',(0.,-0.28578,0.));
#15216=CARTESIAN_POINT('',(-0.980948,-0.166705,1.20131482833E-16));
#15217=CARTESIAN_POINT('',(0.951592097314,-0.04763,0.238183666596899));
#15218=CARTESIAN_POINT('Origin',(0.,-0.04763,0.));
#15219=CARTESIAN_POINT('',(0.951592097314,-0.04763,-0.238183666596899));
#15220=CARTESIAN_POINT('Ctrl Pts',(0.951592097314,-0.04763,0.238183666596899));
#15221=CARTESIAN_POINT('Ctrl Pts',(0.952850216871763,-0.0740444353928835,
0.233157223576062));
#15222=CARTESIAN_POINT('Ctrl Pts',(0.955173119738174,-0.099930567888331,
0.223801617934945));
#15223=CARTESIAN_POINT('Ctrl Pts',(0.960411259488514,-0.142345102874864,
0.199966927975188));
#15224=CARTESIAN_POINT('Ctrl Pts',(0.963103647174702,-0.15976606450048,
0.1868781821531));
#15225=CARTESIAN_POINT('Ctrl Pts',(0.968453058988463,-0.190326085855194,
0.15681442133453));
#15226=CARTESIAN_POINT('Ctrl Pts',(0.971100730005489,-0.203463743702801,
0.139836317888042));
#15227=CARTESIAN_POINT('Ctrl Pts',(0.975530745318961,-0.224161999508995,
0.104422493053067));
#15228=CARTESIAN_POINT('Ctrl Pts',(0.977553872336861,-0.232861760990032,
0.0842175114474172));
#15229=CARTESIAN_POINT('Ctrl Pts',(0.980270995488453,-0.244251601209411,
0.0421062857595697));
#15230=CARTESIAN_POINT('Ctrl Pts',(0.980948,-0.246942143572133,0.0201990724523194));
#15231=CARTESIAN_POINT('Ctrl Pts',(0.980948,-0.246942143572133,-0.0201990724523194));
#15232=CARTESIAN_POINT('Ctrl Pts',(0.980270995488453,-0.244251601209411,
-0.0421062857595697));
#15233=CARTESIAN_POINT('Ctrl Pts',(0.977553872336861,-0.232861760990032,
-0.0842175114474172));
#15234=CARTESIAN_POINT('Ctrl Pts',(0.975530745318961,-0.224161999508995,
-0.104422493053067));
#15235=CARTESIAN_POINT('Ctrl Pts',(0.971100730005489,-0.203463743702801,
-0.139836317888042));
#15236=CARTESIAN_POINT('Ctrl Pts',(0.968453058988463,-0.190326085855194,
-0.15681442133453));
#15237=CARTESIAN_POINT('Ctrl Pts',(0.963103647174702,-0.15976606450048,
-0.1868781821531));
#15238=CARTESIAN_POINT('Ctrl Pts',(0.960411259488514,-0.142345102874864,
-0.199966927975188));
#15239=CARTESIAN_POINT('Ctrl Pts',(0.955173119738174,-0.099930567888331,
-0.223801617934945));
#15240=CARTESIAN_POINT('Ctrl Pts',(0.952850216871763,-0.0740444353928835,
-0.233157223576062));
#15241=CARTESIAN_POINT('Ctrl Pts',(0.951592097314,-0.0476299999999999,-0.238183666596899));
#15242=CARTESIAN_POINT('Origin',(0.,-0.04763,0.));
#15243=CARTESIAN_POINT('Origin',(0.,-0.04763,0.));
#15244=CARTESIAN_POINT('Origin',(1.,-0.04763,0.));
#15245=CARTESIAN_POINT('Origin',(1.,0.,0.));
#15246=CARTESIAN_POINT('Origin',(1.,-0.04763,0.));
#15247=CARTESIAN_POINT('Origin',(0.,-0.28578,0.));
#15248=CARTESIAN_POINT('Origin',(0.,-0.04763,0.));
#15249=CARTESIAN_POINT('',(0.,0.,0.));
#15250=CARTESIAN_POINT('Origin',(1.013815,0.445,0.));
#15251=CARTESIAN_POINT('',(-1.013815,0.445,-1.24156529467757E-16));
#15252=CARTESIAN_POINT('Origin',(0.,0.445,0.));
#15253=CARTESIAN_POINT('',(-0.991185,0.445,-1.21385153761287E-16));
#15254=CARTESIAN_POINT('Origin',(0.,0.445,0.));
#15255=CARTESIAN_POINT('Origin',(0.,0.4075,0.));
#15256=CARTESIAN_POINT('',(-1.013815,0.37,-1.24156529467757E-16));
#15257=CARTESIAN_POINT('Origin',(0.,0.37,0.));
#15258=CARTESIAN_POINT('',(-1.013815,0.4075,-1.24156529467757E-16));
#15259=CARTESIAN_POINT('Origin',(0.991185,0.37,0.));
#15260=CARTESIAN_POINT('',(-0.991185,0.37,-1.21385153761287E-16));
#15261=CARTESIAN_POINT('Origin',(0.,0.37,0.));
#15262=CARTESIAN_POINT('Origin',(0.,0.4075,0.));
#15263=CARTESIAN_POINT('',(-0.991185,0.4075,-1.21385153761287E-16));
#15264=CARTESIAN_POINT('Origin',(1.013815,-0.37,0.));
#15265=CARTESIAN_POINT('',(-1.013815,-0.37,-1.24156529467757E-16));
#15266=CARTESIAN_POINT('Origin',(0.,-0.37,0.));
#15267=CARTESIAN_POINT('',(-0.991185,-0.37,-1.21385153761287E-16));
#15268=CARTESIAN_POINT('Origin',(0.,-0.37,0.));
#15269=CARTESIAN_POINT('Origin',(0.,-0.4075,0.));
#15270=CARTESIAN_POINT('',(-1.013815,-0.445,-1.24156529467757E-16));
#15271=CARTESIAN_POINT('Origin',(0.,-0.445,0.));
#15272=CARTESIAN_POINT('',(-1.013815,-0.4075,-1.24156529467757E-16));
#15273=CARTESIAN_POINT('Origin',(0.991185,-0.445,0.));
#15274=CARTESIAN_POINT('',(-0.991185,-0.445,-1.21385153761287E-16));
#15275=CARTESIAN_POINT('Origin',(0.,-0.445,0.));
#15276=CARTESIAN_POINT('Origin',(0.,-0.4075,0.));
#15277=CARTESIAN_POINT('',(-0.991185,-0.4075,-1.21385153761287E-16));
#15278=CARTESIAN_POINT('',(0.,0.,0.));
#15279=CARTESIAN_POINT('',(0.,0.,0.));
#15280=CARTESIAN_POINT('',(0.,0.,0.));
#15281=CARTESIAN_POINT('',(0.,0.,0.));
#15282=CARTESIAN_POINT('',(0.,0.,0.));
#15283=CARTESIAN_POINT('',(0.,0.,0.));
#15284=CARTESIAN_POINT('Origin',(0.0866025403784439,-0.4,-0.15));
#15285=CARTESIAN_POINT('',(0.173205080756888,-0.4,0.));
#15286=CARTESIAN_POINT('',(0.0866025403784439,-0.4,-0.15));
#15287=CARTESIAN_POINT('',(0.173205080756888,-0.4,0.));
#15288=CARTESIAN_POINT('',(0.0866025403784439,-0.64,-0.15));
#15289=CARTESIAN_POINT('',(0.0866025403784439,-0.4,-0.15));
#15290=CARTESIAN_POINT('',(0.173205080756888,-0.64,0.));
#15291=CARTESIAN_POINT('',(0.173205080756888,-0.64,0.));
#15292=CARTESIAN_POINT('',(0.173205080756888,-0.4,0.));
#15293=CARTESIAN_POINT('Origin',(-0.0866025403784438,-0.4,-0.15));
#15294=CARTESIAN_POINT('',(-0.0866025403784438,-0.4,-0.15));
#15295=CARTESIAN_POINT('',(0.0866025403784439,-0.4,-0.15));
#15296=CARTESIAN_POINT('',(-0.0866025403784438,-0.64,-0.15));
#15297=CARTESIAN_POINT('',(-0.0866025403784438,-0.4,-0.15));
#15298=CARTESIAN_POINT('',(0.0866025403784439,-0.64,-0.15));
#15299=CARTESIAN_POINT('Origin',(-0.173205080756888,-0.4,-2.77555756156289E-17));
#15300=CARTESIAN_POINT('',(-0.173205080756888,-0.4,-2.12115047744981E-17));
#15301=CARTESIAN_POINT('',(-0.0866025403784438,-0.4,-0.15));
#15302=CARTESIAN_POINT('',(-0.173205080756888,-0.64,-2.77555756156289E-17));
#15303=CARTESIAN_POINT('',(-0.173205080756888,-0.4,-2.12115047744981E-17));
#15304=CARTESIAN_POINT('',(-0.0866025403784438,-0.64,-0.15));
#15305=CARTESIAN_POINT('Origin',(-0.0866025403784439,-0.4,0.15));
#15306=CARTESIAN_POINT('',(-0.0866025403784439,-0.4,0.15));
#15307=CARTESIAN_POINT('',(-0.173205080756888,-0.4,-2.12115047744981E-17));
#15308=CARTESIAN_POINT('',(-0.0866025403784439,-0.64,0.15));
#15309=CARTESIAN_POINT('',(-0.0866025403784439,-0.4,0.15));
#15310=CARTESIAN_POINT('',(-0.173205080756888,-0.64,-2.12115047744981E-17));
#15311=CARTESIAN_POINT('Origin',(0.0866025403784439,-0.4,0.15));
#15312=CARTESIAN_POINT('',(0.0866025403784439,-0.4,0.15));
#15313=CARTESIAN_POINT('',(-0.0866025403784439,-0.4,0.15));
#15314=CARTESIAN_POINT('',(0.0866025403784439,-0.64,0.15));
#15315=CARTESIAN_POINT('',(0.0866025403784439,-0.4,0.15));
#15316=CARTESIAN_POINT('',(-0.0866025403784439,-0.64,0.15));
#15317=CARTESIAN_POINT('Origin',(0.173205080756888,-0.4,0.));
#15318=CARTESIAN_POINT('',(0.0866025403784439,-0.4,0.15));
#15319=CARTESIAN_POINT('',(0.0866025403784439,-0.64,0.15));
#15320=CARTESIAN_POINT('Origin',(0.,-0.4,-2.77555756156289E-17));
#15321=CARTESIAN_POINT('Origin',(0.,-0.64,-2.77555756156289E-17));
#15322=CARTESIAN_POINT('Origin',(0.,-1.6,0.));
#15323=CARTESIAN_POINT('',(-0.2,-1.6,2.44929359829471E-17));
#15324=CARTESIAN_POINT('Origin',(0.,-1.6,0.));
#15325=CARTESIAN_POINT('',(-0.16,-1.6,-1.95943487863577E-17));
#15326=CARTESIAN_POINT('Origin',(0.,-1.6,0.));
#15327=CARTESIAN_POINT('Origin',(0.,-3.,0.));
#15328=CARTESIAN_POINT('',(-0.2,-3.,2.44929359829471E-17));
#15329=CARTESIAN_POINT('',(-0.2,-3.,2.44929359829471E-17));
#15330=CARTESIAN_POINT('Origin',(0.,-3.,0.));
#15331=CARTESIAN_POINT('Origin',(0.,-3.,0.));
#15332=CARTESIAN_POINT('Origin',(0.3,0.4,0.));
#15333=CARTESIAN_POINT('',(-0.3,0.4,-3.67394039744206E-17));
#15334=CARTESIAN_POINT('Origin',(0.,0.4,0.));
#15335=CARTESIAN_POINT('Origin',(0.,0.375,0.));
#15336=CARTESIAN_POINT('',(-0.35,0.35,-4.28626379701573E-17));
#15337=CARTESIAN_POINT('Origin',(0.,0.35,0.));
#15338=CARTESIAN_POINT('',(-0.325,0.375,-3.9801020972289E-17));
#15339=CARTESIAN_POINT('Origin',(0.,0.19,0.));
#15340=CARTESIAN_POINT('',(-0.35,0.03,-4.28626379701574E-17));
#15341=CARTESIAN_POINT('Origin',(0.,0.03,0.));
#15342=CARTESIAN_POINT('',(-0.35,0.19,-4.28626379701574E-17));
#15343=CARTESIAN_POINT('Origin',(0.,0.0149999999999999,0.));
#15344=CARTESIAN_POINT('',(-0.32,-3.29597460435593E-17,-3.91886975727153E-17));
#15345=CARTESIAN_POINT('Origin',(0.,0.,0.));
#15346=CARTESIAN_POINT('',(-0.335,0.0149999999999999,-4.10256677714363E-17));
#15347=CARTESIAN_POINT('Origin',(0.22,0.,0.));
#15348=CARTESIAN_POINT('',(-0.22,-6.93889390390723E-18,-2.69422295812418E-17));
#15349=CARTESIAN_POINT('Origin',(0.,0.,0.));
#15350=CARTESIAN_POINT('Origin',(0.,-0.02,0.));
#15351=CARTESIAN_POINT('',(-0.1954,-0.0492,2.39295984553393E-17));
#15352=CARTESIAN_POINT('Origin',(0.,-0.0492,0.));
#15353=CARTESIAN_POINT('',(-0.21,-0.02,-2.57175827820944E-17));
#15354=CARTESIAN_POINT('Origin',(0.,-0.8,0.));
#15355=CARTESIAN_POINT('',(-0.1954,-1.5646,2.39295984553393E-17));
#15356=CARTESIAN_POINT('Origin',(0.,-1.5646,0.));
#15357=CARTESIAN_POINT('',(-0.1954,-0.8,-2.39295984553393E-17));
#15358=CARTESIAN_POINT('Origin',(0.,-1.58,0.));
#15359=CARTESIAN_POINT('',(-0.18,-1.58,-2.20436423846524E-17));
#15360=CARTESIAN_POINT('',(0.,0.,0.));
#15361=CARTESIAN_POINT('',(0.,0.,0.));
#15362=CARTESIAN_POINT('Origin',(0.,0.,0.));
#15363=CARTESIAN_POINT('',(-1.070235,-0.308121667383195,-1.31065986708547E-16));
#15364=CARTESIAN_POINT('',(-1.31065986708547E-16,-0.308121667383195,1.070235));
#15365=CARTESIAN_POINT('Origin',(0.,-0.308121667383195,0.));
#15366=CARTESIAN_POINT('Origin',(0.,-0.308121667383195,0.));
#15367=CARTESIAN_POINT('',(-1.31065986708547E-16,0.308121667383195,1.070235));
#15368=CARTESIAN_POINT('Origin',(-1.34711147906209E-16,0.,1.1));
#15369=CARTESIAN_POINT('',(-1.070235,0.308121667383195,1.31065986708547E-16));
#15370=CARTESIAN_POINT('Origin',(0.,0.308121667383195,0.));
#15371=CARTESIAN_POINT('Origin',(0.,0.308121667383195,0.));
#15372=CARTESIAN_POINT('Origin',(0.,0.,0.));
#15373=CARTESIAN_POINT('',(-1.070235,0.5,-1.31065986708547E-16));
#15374=CARTESIAN_POINT('',(-1.070235,0.,-1.31065986708547E-16));
#15375=CARTESIAN_POINT('Origin',(0.,0.5,0.));
#15376=CARTESIAN_POINT('Origin',(0.,0.,0.));
#15377=CARTESIAN_POINT('',(-0.6,-0.44,-7.34788079488412E-17));
#15378=CARTESIAN_POINT('Origin',(0.,-0.44,0.));
#15379=CARTESIAN_POINT('',(-0.6,0.44,-7.34788079488412E-17));
#15380=CARTESIAN_POINT('',(-0.6,0.,-7.34788079488412E-17));
#15381=CARTESIAN_POINT('Origin',(0.,0.44,0.));
#15382=CARTESIAN_POINT('Origin',(0.,0.47,0.));
#15383=CARTESIAN_POINT('',(-0.66,0.5,-8.08266887437253E-17));
#15384=CARTESIAN_POINT('',(-0.63,0.47,-7.71527483462832E-17));
#15385=CARTESIAN_POINT('Origin',(0.,0.5,0.));
#15386=CARTESIAN_POINT('Origin',(1.070235,0.5,0.));
#15387=CARTESIAN_POINT('Origin',(0.,0.,0.));
#15388=CARTESIAN_POINT('',(-1.070235,-0.5,-1.31065986708547E-16));
#15389=CARTESIAN_POINT('Origin',(0.,-0.5,0.));
#15390=CARTESIAN_POINT('',(-1.070235,0.,-1.31065986708547E-16));
#15391=CARTESIAN_POINT('Origin',(0.66,-0.5,0.));
#15392=CARTESIAN_POINT('',(-0.66,-0.5,-8.08266887437253E-17));
#15393=CARTESIAN_POINT('Origin',(0.,-0.5,0.));
#15394=CARTESIAN_POINT('Origin',(0.,-0.47,0.));
#15395=CARTESIAN_POINT('',(-0.63,-0.47,-7.71527483462832E-17));
#15396=CARTESIAN_POINT('',(0.,0.,0.));
#15397=CARTESIAN_POINT('Origin',(0.,0.,0.));
#15398=CARTESIAN_POINT('',(-1.129765,0.308121667383195,-1.38356309103871E-16));
#15399=CARTESIAN_POINT('',(-1.38356309103871E-16,0.308121667383195,1.129765));
#15400=CARTESIAN_POINT('Origin',(0.,0.308121667383195,0.));
#15401=CARTESIAN_POINT('Origin',(0.,0.308121667383195,0.));
#15402=CARTESIAN_POINT('',(-1.38356309103871E-16,-0.308121667383195,1.129765));
#15403=CARTESIAN_POINT('Origin',(-1.34711147906209E-16,0.,1.1));
#15404=CARTESIAN_POINT('',(-1.129765,-0.308121667383195,1.38356309103871E-16));
#15405=CARTESIAN_POINT('Origin',(0.,-0.308121667383195,0.));
#15406=CARTESIAN_POINT('Origin',(0.,-0.308121667383195,0.));
#15407=CARTESIAN_POINT('Origin',(0.,0.,0.));
#15408=CARTESIAN_POINT('',(-1.129765,-0.5,-1.38356309103871E-16));
#15409=CARTESIAN_POINT('Origin',(0.,-0.5,0.));
#15410=CARTESIAN_POINT('',(-1.129765,0.,-1.38356309103871E-16));
#15411=CARTESIAN_POINT('Origin',(1.54,0.5,0.));
#15412=CARTESIAN_POINT('',(-1.54,0.5,-1.88595607068692E-16));
#15413=CARTESIAN_POINT('Origin',(0.,0.5,0.));
#15414=CARTESIAN_POINT('',(-1.129765,0.5,-1.38356309103871E-16));
#15415=CARTESIAN_POINT('Origin',(0.,0.5,0.));
#15416=CARTESIAN_POINT('Origin',(0.,0.47,0.));
#15417=CARTESIAN_POINT('',(-1.6,0.44,-1.95943487863577E-16));
#15418=CARTESIAN_POINT('Origin',(0.,0.44,0.));
#15419=CARTESIAN_POINT('',(-1.57,0.47,-1.92269547466134E-16));
#15420=CARTESIAN_POINT('Origin',(0.,0.,0.));
#15421=CARTESIAN_POINT('',(-1.6,-0.44,-1.95943487863577E-16));
#15422=CARTESIAN_POINT('Origin',(0.,-0.44,0.));
#15423=CARTESIAN_POINT('',(-1.6,0.,-1.95943487863577E-16));
#15424=CARTESIAN_POINT('Origin',(0.,-0.47,0.));
#15425=CARTESIAN_POINT('',(-1.54,-0.5,-1.88595607068692E-16));
#15426=CARTESIAN_POINT('Origin',(0.,-0.5,0.));
#15427=CARTESIAN_POINT('',(-1.57,-0.47,-1.92269547466134E-16));
#15428=CARTESIAN_POINT('Origin',(1.129765,-0.5,0.));
#15429=CARTESIAN_POINT('Origin',(0.,0.,0.));
#15430=CARTESIAN_POINT('',(-1.129765,0.,-1.38356309103871E-16));
#15431=CARTESIAN_POINT('',(0.,0.,0.));
#15432=CARTESIAN_POINT('Origin',(1.1,0.,0.));
#15433=CARTESIAN_POINT('',(1.1,-2.23201749654651E-33,0.29765));
#15434=CARTESIAN_POINT('',(1.1,-2.23201749654651E-33,-0.29765));
#15435=CARTESIAN_POINT('Origin',(1.1,0.,0.));
#15436=CARTESIAN_POINT('Origin',(0.685838782044607,0.,-0.860014630714833));
#15437=CARTESIAN_POINT('',(0.918550922801216,-5.31350540756609E-33,-0.674432891191581));
#15438=CARTESIAN_POINT('',(0.453126641287998,8.49470414473068E-34,-1.04559637023808));
#15439=CARTESIAN_POINT('Origin',(0.685838782044607,0.,-0.860014630714833));
#15440=CARTESIAN_POINT('Origin',(-0.244773027351946,0.,-1.07242070340001));
#15441=CARTESIAN_POINT('',(0.0454142657089739,-2.23201749654651E-33,-1.1386540593921));
#15442=CARTESIAN_POINT('',(-0.534960320412865,-2.23201749654651E-33,-1.00618734740791));
#15443=CARTESIAN_POINT('Origin',(-0.244773027351946,0.,-1.07242070340001));
#15444=CARTESIAN_POINT('Origin',(-0.991065754692661,0.,-0.477272113029314));
#15445=CARTESIAN_POINT('',(-0.86192025974432,8.49470414473067E-34,-0.745445496560469));
#15446=CARTESIAN_POINT('',(-1.120211249641,-5.31350540756609E-33,-0.209098729498159));
#15447=CARTESIAN_POINT('Origin',(-0.991065754692661,0.,-0.477272113029314));
#15448=CARTESIAN_POINT('Origin',(-0.991065754692661,0.,0.477272113029314));
#15449=CARTESIAN_POINT('',(-1.120211249641,-2.23201749654651E-33,0.209098729498159));
#15450=CARTESIAN_POINT('',(-0.86192025974432,-2.23201749654651E-33,0.745445496560469));
#15451=CARTESIAN_POINT('Origin',(-0.991065754692661,0.,0.477272113029314));
#15452=CARTESIAN_POINT('Origin',(-0.244773027351946,0.,1.07242070340001));
#15453=CARTESIAN_POINT('',(-0.534960320412866,-2.23201749654651E-33,1.00618734740791));
#15454=CARTESIAN_POINT('',(0.0454142657089737,-2.23201749654651E-33,1.1386540593921));
#15455=CARTESIAN_POINT('Origin',(-0.244773027351946,0.,1.07242070340001));
#15456=CARTESIAN_POINT('Origin',(0.685838782044607,0.,0.860014630714833));
#15457=CARTESIAN_POINT('',(0.453126641287998,-2.23201749654651E-33,1.04559637023808));
#15458=CARTESIAN_POINT('',(0.918550922801216,-2.23201749654651E-33,0.674432891191581));
#15459=CARTESIAN_POINT('Origin',(0.685838782044607,0.,0.860014630714833));
#15460=CARTESIAN_POINT('',(0.,0.,0.));
#15461=CARTESIAN_POINT('Origin',(0.685838782044607,0.,0.860014630714833));
#15462=CARTESIAN_POINT('',(0.413083465285518,-0.05953,0.993751811093549));
#15463=CARTESIAN_POINT('',(0.876916659919095,-0.05953,0.623857181492959));
#15464=CARTESIAN_POINT('Ctrl Pts',(0.413083465285518,-0.05953,0.993751811093549));
#15465=CARTESIAN_POINT('Ctrl Pts',(0.419070565453383,-0.0925528133349865,
0.991263089003441));
#15466=CARTESIAN_POINT('Ctrl Pts',(0.430199341854858,-0.124911173756694,
0.986608710139579));
#15467=CARTESIAN_POINT('Ctrl Pts',(0.457978755888596,-0.177924977804098,
0.973971221090534));
#15468=CARTESIAN_POINT('Ctrl Pts',(0.473077587363685,-0.199697230012983,
0.966820759530997));
#15469=CARTESIAN_POINT('Ctrl Pts',(0.507057380724533,-0.237895043532788,
0.949440676105255));
#15470=CARTESIAN_POINT('Ctrl Pts',(0.525933334162555,-0.254319232363049,
0.939198248544428));
#15471=CARTESIAN_POINT('Ctrl Pts',(0.564362943424238,-0.28018331644634,
0.916597376014514));
#15472=CARTESIAN_POINT('Ctrl Pts',(0.585840553788742,-0.29104845371857,
0.903141581680914));
#15473=CARTESIAN_POINT('Ctrl Pts',(0.629305439856167,-0.30527573347708,
0.873412008702649));
#15474=CARTESIAN_POINT('Ctrl Pts',(0.651278921914856,-0.308638795020976,
0.857118508332695));
#15475=CARTESIAN_POINT('Ctrl Pts',(0.690705563850638,-0.308638795020976,
0.825676810575914));
#15476=CARTESIAN_POINT('Ctrl Pts',(0.711480111898423,-0.30527573347708,
0.807879894508811));
#15477=CARTESIAN_POINT('Ctrl Pts',(0.750136149454208,-0.29104845371857,
0.772120216227122));
#15478=CARTESIAN_POINT('Ctrl Pts',(0.768033796848072,-0.28018331644634,
0.754175290318038));
#15479=CARTESIAN_POINT('Ctrl Pts',(0.798619410861634,-0.254319232363049,
0.721738358858166));
#15480=CARTESIAN_POINT('Ctrl Pts',(0.812805334167529,-0.237895043532788,
0.705614819529209));
#15481=CARTESIAN_POINT('Ctrl Pts',(0.837310877969633,-0.199697230012983,
0.676354402927683));
#15482=CARTESIAN_POINT('Ctrl Pts',(0.847641868610495,-0.177924977804098,
0.663225258065736));
#15483=CARTESIAN_POINT('Ctrl Pts',(0.866144010579847,-0.124911173756694,
0.638954437806245));
#15484=CARTESIAN_POINT('Ctrl Pts',(0.873158080166742,-0.0925528133349865,
0.62914037979579));
#15485=CARTESIAN_POINT('Ctrl Pts',(0.876916659919095,-0.05953,0.623857181492959));
#15486=CARTESIAN_POINT('',(0.437601487681057,-0.05953,1.03511272300331));
#15487=CARTESIAN_POINT('Origin',(0.685838782044607,-0.05953,0.860014630714833));
#15488=CARTESIAN_POINT('',(0.911784794170997,-0.05953,0.656964154625313));
#15489=CARTESIAN_POINT('Ctrl Pts',(0.911784794170998,-0.0595300000000001,
0.656964154625312));
#15490=CARTESIAN_POINT('Ctrl Pts',(0.909827729890942,-0.0762225747374255,
0.659680317203144));
#15491=CARTESIAN_POINT('Ctrl Pts',(0.907004864562642,-0.0928409665394228,
0.663576540841106));
#15492=CARTESIAN_POINT('Ctrl Pts',(0.895234408667242,-0.144299303100741,
0.679480524217551));
#15493=CARTESIAN_POINT('Ctrl Pts',(0.882797231409153,-0.177024326825049,
0.695831250979106));
#15494=CARTESIAN_POINT('Ctrl Pts',(0.854332839576145,-0.227269801620064,
0.73042219438957));
#15495=CARTESIAN_POINT('Ctrl Pts',(0.834863020612702,-0.251265615809407,
0.752807465209441));
#15496=CARTESIAN_POINT('Ctrl Pts',(0.800439809856111,-0.279889827963178,
0.789147407129766));
#15497=CARTESIAN_POINT('Ctrl Pts',(0.781998747691871,-0.290879136862659,
0.80756613568454));
#15498=CARTESIAN_POINT('Ctrl Pts',(0.742239891936898,-0.305251990234487,
0.844254137480382));
#15499=CARTESIAN_POINT('Ctrl Pts',(0.720906778729541,-0.308638795020976,
0.862505527716294));
#15500=CARTESIAN_POINT('Ctrl Pts',(0.680463863683392,-0.308638795020976,
0.894757676234429));
#15501=CARTESIAN_POINT('Ctrl Pts',(0.657923009631182,-0.305251990234488,
0.91149460735272));
#15502=CARTESIAN_POINT('Ctrl Pts',(0.613307674922609,-0.290879136862659,
0.942092777160053));
#15503=CARTESIAN_POINT('Ctrl Pts',(0.591247219971725,-0.279889827963178,
0.955972930713954));
#15504=CARTESIAN_POINT('Ctrl Pts',(0.548158511259202,-0.251265615809407,
0.981446681891443));
#15505=CARTESIAN_POINT('Ctrl Pts',(0.522002043615455,-0.227269801620063,
0.995447160474328));
#15506=CARTESIAN_POINT('Ctrl Pts',(0.481944444320713,-0.177024326825049,
1.01550068154148));
#15507=CARTESIAN_POINT('Ctrl Pts',(0.463236132117164,-0.14429930310074,
1.0239876538093));
#15508=CARTESIAN_POINT('Ctrl Pts',(0.445111721969657,-0.0928409665394226,
1.03192403056628));
#15509=CARTESIAN_POINT('Ctrl Pts',(0.440685038163619,-0.0762225747374254,
1.03380912944435));
#15510=CARTESIAN_POINT('Ctrl Pts',(0.437601487681056,-0.05953,1.03511272300331));
#15511=CARTESIAN_POINT('Origin',(0.685838782044607,-0.05953,0.860014630714833));
#15512=CARTESIAN_POINT('Origin',(0.,-0.208355,0.));
#15513=CARTESIAN_POINT('',(0.0548532617164168,-0.05953,1.12247250791415));
#15514=CARTESIAN_POINT('Origin',(0.,-0.05953,0.));
#15515=CARTESIAN_POINT('',(-0.536443649899848,-0.05953,0.987512846410683));
#15516=CARTESIAN_POINT('Ctrl Pts',(0.0548532617164173,-0.0595300000000001,
1.12247250791414));
#15517=CARTESIAN_POINT('Ctrl Pts',(0.05150947068137,-0.0762225747374254,
1.12263591311425));
#15518=CARTESIAN_POINT('Ctrl Pts',(0.0467032526342597,-0.0928409665394227,
1.12285816383385));
#15519=CARTESIAN_POINT('Ctrl Pts',(0.0269302585198975,-0.144299303100741,
1.12357162229597));
#15520=CARTESIAN_POINT('Ctrl Pts',(0.006392292392153,-0.177024326825049,
1.12404235695137));
#15521=CARTESIAN_POINT('Ctrl Pts',(-0.0383992541984087,-0.227269801620063,
1.12335509974011));
#15522=CARTESIAN_POINT('Ctrl Pts',(-0.0680399972366993,-0.251265615809407,
1.12208997038458));
#15523=CARTESIAN_POINT('Ctrl Pts',(-0.117914228755037,-0.279889827963178,
1.1178344036749));
#15524=CARTESIAN_POINT('Ctrl Pts',(-0.14381238480104,-0.290879136862659,
1.11490049012186));
#15525=CARTESIAN_POINT('Ctrl Pts',(-0.19728546073067,-0.305251990234488,
1.10669035995599));
#15526=CARTESIAN_POINT('Ctrl Pts',(-0.224855950742601,-0.308638795020976,
1.10139101611326));
#15527=CARTESIAN_POINT('Ctrl Pts',(-0.275287440920027,-0.308638795020976,
1.0898803575765));
#15528=CARTESIAN_POINT('Ctrl Pts',(-0.302426893214945,-0.305251990234488,
1.08269251410343));
#15529=CARTESIAN_POINT('Ctrl Pts',(-0.35416671187353,-0.290879136862659,
1.06688848765783));
#15530=CARTESIAN_POINT('Ctrl Pts',(-0.3787731215897,-0.279889827963178,
1.05829506364875));
#15531=CARTESIAN_POINT('Ctrl Pts',(-0.425554672694338,-0.251265615809407,
1.04048957871266));
#15532=CARTESIAN_POINT('Ctrl Pts',(-0.452808978448581,-0.227269801620063,
1.02876878445619));
#15533=CARTESIAN_POINT('Ctrl Pts',(-0.493462957200432,-0.177024326825049,
1.0099536580922));
#15534=CARTESIAN_POINT('Ctrl Pts',(-0.511762781179148,-0.14429930310074,
1.00061845128527));
#15535=CARTESIAN_POINT('Ctrl Pts',(-0.529268075276157,-0.0928409665394226,
0.991396466802468));
#15536=CARTESIAN_POINT('Ctrl Pts',(-0.533501897135713,-0.0762225747374254,
0.989110885965947));
#15537=CARTESIAN_POINT('Ctrl Pts',(-0.536443649899848,-0.0595300000000001,
0.987512846410683));
#15538=CARTESIAN_POINT('',(-0.843383895613249,-0.05953,0.742736168477219));
#15539=CARTESIAN_POINT('Origin',(0.,-0.05953,0.));
#15540=CARTESIAN_POINT('',(-1.10653577764992,-0.05953,0.196295654879792));
#15541=CARTESIAN_POINT('Ctrl Pts',(-0.843383895613249,-0.0595300000000001,
0.742736168477219));
#15542=CARTESIAN_POINT('Ctrl Pts',(-0.84559647055299,-0.0762225747374255,
0.740223768851062));
#15543=CARTESIAN_POINT('Ctrl Pts',(-0.848766861100456,-0.0928409665394227,
0.736604687327351));
#15544=CARTESIAN_POINT('Ctrl Pts',(-0.861652925570091,-0.144299303100741,
0.721590372101268));
#15545=CARTESIAN_POINT('Ctrl Pts',(-0.87482617317514,-0.177024326825049,
0.705826641853758));
#15546=CARTESIAN_POINT('Ctrl Pts',(-0.902215926359523,-0.227269801620063,
0.670378702718353));
#15547=CARTESIAN_POINT('Ctrl Pts',(-0.919707509403859,-0.251265615809407,
0.646415841396062));
#15548=CARTESIAN_POINT('Ctrl Pts',(-0.947476448101718,-0.279889827963178,
0.604769294586516));
#15549=CARTESIAN_POINT('Ctrl Pts',(-0.961329858300736,-0.290879136862659,
0.582692035672022));
#15550=CARTESIAN_POINT('Ctrl Pts',(-0.988250837578047,-0.305251990234488,
0.535766169015486));
#15551=CARTESIAN_POINT('Ctrl Pts',(-1.00129756308006,-0.308638795020976,
0.510906605094603));
#15552=CARTESIAN_POINT('Ctrl Pts',(-1.02374168767024,-0.308638795020976,
0.46430090015576));
#15553=CARTESIAN_POINT('Ctrl Pts',(-1.03504317708586,-0.305251990234488,
0.438600874831839));
#15554=CARTESIAN_POINT('Ctrl Pts',(-1.05494634094458,-0.290879136862659,
0.388295406390235));
#15555=CARTESIAN_POINT('Ctrl Pts',(-1.06356957703048,-0.279889827963178,
0.363699428370917));
#15556=CARTESIAN_POINT('Ctrl Pts',(-1.0788165083757,-0.251265615809407,
0.316022600643821));
#15557=CARTESIAN_POINT('Ctrl Pts',(-1.08664560412098,-0.227269801620063,
0.287406530683752));
#15558=CARTESIAN_POINT('Ctrl Pts',(-1.09728268713976,-0.177024326825049,
0.243890930799337));
#15559=CARTESIAN_POINT('Ctrl Pts',(-1.10139388218929,-0.144299303100741,
0.22376314604679));
#15560=CARTESIAN_POINT('Ctrl Pts',(-1.10509821673782,-0.0928409665394227,
0.204327142733961));
#15561=CARTESIAN_POINT('Ctrl Pts',(-1.10595102243643,-0.0762225747374254,
0.199591971170104));
#15562=CARTESIAN_POINT('Ctrl Pts',(-1.10653577764992,-0.0595300000000001,
0.196295654879792));
#15563=CARTESIAN_POINT('',(-1.123812,-0.05953,1.37627276864339E-16));
#15564=CARTESIAN_POINT('Origin',(0.,-0.05953,0.));
#15565=CARTESIAN_POINT('',(-1.123812,-0.35718,1.37627276864339E-16));
#15566=CARTESIAN_POINT('',(-1.123812,-0.208355,1.37627276864339E-16));
#15567=CARTESIAN_POINT('Origin',(0.,-0.35718,0.));
#15568=CARTESIAN_POINT('',(-1.10653577764992,-0.05953,-0.196295654879793));
#15569=CARTESIAN_POINT('Origin',(0.,-0.05953,0.));
#15570=CARTESIAN_POINT('',(-0.843383895613249,-0.05953,-0.742736168477219));
#15571=CARTESIAN_POINT('Ctrl Pts',(-1.10653577764992,-0.0595300000000001,
-0.196295654879792));
#15572=CARTESIAN_POINT('Ctrl Pts',(-1.10595102243643,-0.0762225747374255,
-0.199591971170104));
#15573=CARTESIAN_POINT('Ctrl Pts',(-1.10509821673782,-0.0928409665394228,
-0.204327142733962));
#15574=CARTESIAN_POINT('Ctrl Pts',(-1.10139388218929,-0.144299303100741,
-0.22376314604679));
#15575=CARTESIAN_POINT('Ctrl Pts',(-1.09728268713976,-0.177024326825049,
-0.243890930799338));
#15576=CARTESIAN_POINT('Ctrl Pts',(-1.08664560412098,-0.227269801620063,
-0.287406530683753));
#15577=CARTESIAN_POINT('Ctrl Pts',(-1.0788165083757,-0.251265615809407,
-0.316022600643821));
#15578=CARTESIAN_POINT('Ctrl Pts',(-1.06356957703048,-0.279889827963178,
-0.363699428370918));
#15579=CARTESIAN_POINT('Ctrl Pts',(-1.05494634094458,-0.290879136862659,
-0.388295406390235));
#15580=CARTESIAN_POINT('Ctrl Pts',(-1.03504317708586,-0.305251990234488,
-0.438600874831839));
#15581=CARTESIAN_POINT('Ctrl Pts',(-1.02374168767024,-0.308638795020976,
-0.46430090015576));
#15582=CARTESIAN_POINT('Ctrl Pts',(-1.00129756308006,-0.308638795020976,
-0.510906605094603));
#15583=CARTESIAN_POINT('Ctrl Pts',(-0.988250837578047,-0.305251990234488,
-0.535766169015486));
#15584=CARTESIAN_POINT('Ctrl Pts',(-0.961329858300736,-0.290879136862659,
-0.582692035672022));
#15585=CARTESIAN_POINT('Ctrl Pts',(-0.947476448101718,-0.279889827963178,
-0.604769294586516));
#15586=CARTESIAN_POINT('Ctrl Pts',(-0.919707509403859,-0.251265615809407,
-0.646415841396062));
#15587=CARTESIAN_POINT('Ctrl Pts',(-0.902215926359523,-0.227269801620064,
-0.670378702718353));
#15588=CARTESIAN_POINT('Ctrl Pts',(-0.87482617317514,-0.177024326825049,
-0.705826641853758));
#15589=CARTESIAN_POINT('Ctrl Pts',(-0.861652925570091,-0.144299303100741,
-0.721590372101268));
#15590=CARTESIAN_POINT('Ctrl Pts',(-0.848766861100456,-0.0928409665394229,
-0.736604687327351));
#15591=CARTESIAN_POINT('Ctrl Pts',(-0.84559647055299,-0.0762225747374255,
-0.740223768851063));
#15592=CARTESIAN_POINT('Ctrl Pts',(-0.843383895613249,-0.0595300000000001,
-0.742736168477219));
#15593=CARTESIAN_POINT('',(-0.536443649899847,-0.05953,-0.987512846410683));
#15594=CARTESIAN_POINT('Origin',(0.,-0.05953,0.));
#15595=CARTESIAN_POINT('',(0.0548532617164172,-0.05953,-1.12247250791415));
#15596=CARTESIAN_POINT('Ctrl Pts',(-0.536443649899848,-0.0595300000000001,
-0.987512846410683));
#15597=CARTESIAN_POINT('Ctrl Pts',(-0.533501897135712,-0.0762225747374254,
-0.989110885965947));
#15598=CARTESIAN_POINT('Ctrl Pts',(-0.529268075276156,-0.0928409665394227,
-0.991396466802469));
#15599=CARTESIAN_POINT('Ctrl Pts',(-0.511762781179147,-0.144299303100741,
-1.00061845128527));
#15600=CARTESIAN_POINT('Ctrl Pts',(-0.493462957200432,-0.177024326825049,
-1.0099536580922));
#15601=CARTESIAN_POINT('Ctrl Pts',(-0.45280897844858,-0.227269801620063,
-1.02876878445619));
#15602=CARTESIAN_POINT('Ctrl Pts',(-0.425554672694337,-0.251265615809407,
-1.04048957871266));
#15603=CARTESIAN_POINT('Ctrl Pts',(-0.3787731215897,-0.279889827963178,
-1.05829506364875));
#15604=CARTESIAN_POINT('Ctrl Pts',(-0.354166711873529,-0.290879136862659,
-1.06688848765783));
#15605=CARTESIAN_POINT('Ctrl Pts',(-0.302426893214944,-0.305251990234488,
-1.08269251410343));
#15606=CARTESIAN_POINT('Ctrl Pts',(-0.275287440920027,-0.308638795020976,
-1.0898803575765));
#15607=CARTESIAN_POINT('Ctrl Pts',(-0.224855950742601,-0.308638795020976,
-1.10139101611326));
#15608=CARTESIAN_POINT('Ctrl Pts',(-0.19728546073067,-0.305251990234488,
-1.10669035995599));
#15609=CARTESIAN_POINT('Ctrl Pts',(-0.143812384801039,-0.290879136862659,
-1.11490049012186));
#15610=CARTESIAN_POINT('Ctrl Pts',(-0.117914228755037,-0.279889827963178,
-1.1178344036749));
#15611=CARTESIAN_POINT('Ctrl Pts',(-0.0680399972366989,-0.251265615809407,
-1.12208997038458));
#15612=CARTESIAN_POINT('Ctrl Pts',(-0.0383992541984084,-0.227269801620063,
-1.12335509974011));
#15613=CARTESIAN_POINT('Ctrl Pts',(0.00639229239215326,-0.177024326825049,
-1.12404235695137));
#15614=CARTESIAN_POINT('Ctrl Pts',(0.0269302585198977,-0.144299303100741,
-1.12357162229597));
#15615=CARTESIAN_POINT('Ctrl Pts',(0.04670325263426,-0.0928409665394228,
-1.12285816383385));
#15616=CARTESIAN_POINT('Ctrl Pts',(0.0515094706813703,-0.0762225747374255,
-1.12263591311425));
#15617=CARTESIAN_POINT('Ctrl Pts',(0.0548532617164176,-0.0595300000000001,
-1.12247250791414));
#15618=CARTESIAN_POINT('',(0.437601487681057,-0.05953,-1.03511272300331));
#15619=CARTESIAN_POINT('Origin',(0.,-0.05953,0.));
#15620=CARTESIAN_POINT('',(0.911784794170997,-0.05953,-0.656964154625313));
#15621=CARTESIAN_POINT('Ctrl Pts',(0.437601487681056,-0.0595300000000001,
-1.03511272300331));
#15622=CARTESIAN_POINT('Ctrl Pts',(0.440685038163619,-0.0762225747374255,
-1.03380912944435));
#15623=CARTESIAN_POINT('Ctrl Pts',(0.445111721969657,-0.0928409665394228,
-1.03192403056628));
#15624=CARTESIAN_POINT('Ctrl Pts',(0.463236132117164,-0.144299303100741,
-1.0239876538093));
#15625=CARTESIAN_POINT('Ctrl Pts',(0.481944444320713,-0.177024326825049,
-1.01550068154148));
#15626=CARTESIAN_POINT('Ctrl Pts',(0.522002043615455,-0.227269801620064,
-0.995447160474328));
#15627=CARTESIAN_POINT('Ctrl Pts',(0.548158511259203,-0.251265615809407,
-0.981446681891443));
#15628=CARTESIAN_POINT('Ctrl Pts',(0.591247219971725,-0.279889827963178,
-0.955972930713954));
#15629=CARTESIAN_POINT('Ctrl Pts',(0.613307674922609,-0.290879136862659,
-0.942092777160053));
#15630=CARTESIAN_POINT('Ctrl Pts',(0.657923009631182,-0.305251990234487,
-0.91149460735272));
#15631=CARTESIAN_POINT('Ctrl Pts',(0.680463863683393,-0.308638795020976,
-0.894757676234429));
#15632=CARTESIAN_POINT('Ctrl Pts',(0.720906778729542,-0.308638795020976,
-0.862505527716294));
#15633=CARTESIAN_POINT('Ctrl Pts',(0.742239891936899,-0.305251990234488,
-0.844254137480381));
#15634=CARTESIAN_POINT('Ctrl Pts',(0.781998747691872,-0.290879136862659,
-0.80756613568454));
#15635=CARTESIAN_POINT('Ctrl Pts',(0.800439809856112,-0.279889827963178,
-0.789147407129765));
#15636=CARTESIAN_POINT('Ctrl Pts',(0.834863020612702,-0.251265615809407,
-0.752807465209441));
#15637=CARTESIAN_POINT('Ctrl Pts',(0.854332839576145,-0.227269801620064,
-0.73042219438957));
#15638=CARTESIAN_POINT('Ctrl Pts',(0.882797231409153,-0.177024326825049,
-0.695831250979106));
#15639=CARTESIAN_POINT('Ctrl Pts',(0.895234408667242,-0.144299303100741,
-0.679480524217551));
#15640=CARTESIAN_POINT('Ctrl Pts',(0.907004864562642,-0.0928409665394228,
-0.663576540841106));
#15641=CARTESIAN_POINT('Ctrl Pts',(0.909827729890942,-0.0762225747374256,
-0.659680317203144));
#15642=CARTESIAN_POINT('Ctrl Pts',(0.911784794170998,-0.0595300000000001,
-0.656964154625312));
#15643=CARTESIAN_POINT('',(1.08212377959455,-0.05953,-0.303251606722892));
#15644=CARTESIAN_POINT('Origin',(0.,-0.05953,0.));
#15645=CARTESIAN_POINT('',(1.08212377959455,-0.05953,0.303251606722892));
#15646=CARTESIAN_POINT('Ctrl Pts',(1.08212377959455,-0.0595300000000001,
-0.303251606722892));
#15647=CARTESIAN_POINT('Ctrl Pts',(1.0830271513892,-0.0762225747374255,
-0.300028012588062));
#15648=CARTESIAN_POINT('Ctrl Pts',(1.08431331394788,-0.0928409665394228,
-0.2953917518996));
#15649=CARTESIAN_POINT('Ctrl Pts',(1.08940878963422,-0.144299303100741,
-0.276273267473431));
#15650=CARTESIAN_POINT('Ctrl Pts',(1.09443784939331,-0.177024326825049,
-0.256354979351213));
#15651=CARTESIAN_POINT('Ctrl Pts',(1.10373487993589,-0.227269801620064,
-0.212533521233765));
#15652=CARTESIAN_POINT('Ctrl Pts',(1.10909715583869,-0.251265615809407,
-0.183354415742157));
#15653=CARTESIAN_POINT('Ctrl Pts',(1.1160463456491,-0.279889827963178,-0.133783682657561));
#15654=CARTESIAN_POINT('Ctrl Pts',(1.11894887330541,-0.290879136862659,
-0.107881990270302));
#15655=CARTESIAN_POINT('Ctrl Pts',(1.12284346704144,-0.305251990234488,
-0.0539226701638766));
#15656=CARTESIAN_POINT('Ctrl Pts',(1.123812,-0.308638795020976,-0.025864214957475));
#15657=CARTESIAN_POINT('Ctrl Pts',(1.123812,-0.308638795020976,0.025864214957475));
#15658=CARTESIAN_POINT('Ctrl Pts',(1.12284346704144,-0.305251990234488,
0.0539226701638766));
#15659=CARTESIAN_POINT('Ctrl Pts',(1.11894887330541,-0.290879136862659,
0.107881990270302));
#15660=CARTESIAN_POINT('Ctrl Pts',(1.1160463456491,-0.279889827963178,0.133783682657561));
#15661=CARTESIAN_POINT('Ctrl Pts',(1.10909715583869,-0.251265615809407,
0.183354415742157));
#15662=CARTESIAN_POINT('Ctrl Pts',(1.10373487993589,-0.227269801620064,
0.212533521233765));
#15663=CARTESIAN_POINT('Ctrl Pts',(1.09443784939331,-0.177024326825049,
0.256354979351213));
#15664=CARTESIAN_POINT('Ctrl Pts',(1.08940878963422,-0.144299303100741,
0.276273267473431));
#15665=CARTESIAN_POINT('Ctrl Pts',(1.08431331394788,-0.0928409665394228,
0.2953917518996));
#15666=CARTESIAN_POINT('Ctrl Pts',(1.0830271513892,-0.0762225747374255,
0.300028012588062));
#15667=CARTESIAN_POINT('Ctrl Pts',(1.08212377959455,-0.0595300000000001,
0.303251606722892));
#15668=CARTESIAN_POINT('Origin',(0.,-0.05953,0.));
#15669=CARTESIAN_POINT('Origin',(0.,-0.05953,0.));
#15670=CARTESIAN_POINT('',(0.0589974094846122,-0.05953,1.07456964270265));
#15671=CARTESIAN_POINT('Origin',(0.,-0.05953,0.));
#15672=CARTESIAN_POINT('Origin',(-0.244773027351946,-0.05953,1.07242070340001));
#15673=CARTESIAN_POINT('Origin',(-0.244773027351946,0.,1.07242070340001));
#15674=CARTESIAN_POINT('',(-0.519393123750572,-0.05953,0.942555777842682));
#15675=CARTESIAN_POINT('Ctrl Pts',(-0.519393123750572,-0.05953,0.942555777842682));
#15676=CARTESIAN_POINT('Ctrl Pts',(-0.513714466572041,-0.0925528133349865,
0.945684988399766));
#15677=CARTESIAN_POINT('Ctrl Pts',(-0.503136848051455,-0.124911173756694,
0.951483858396181));
#15678=CARTESIAN_POINT('Ctrl Pts',(-0.47593627990192,-0.177924977804098,
0.965323333309091));
#15679=CARTESIAN_POINT('Ctrl Pts',(-0.460931856495794,-0.199697230012983,
0.972669835243841));
#15680=CARTESIAN_POINT('Ctrl Pts',(-0.426157505475872,-0.237895043532788,
0.988400002689705));
#15681=CARTESIAN_POINT('Ctrl Pts',(-0.406380688682952,-0.254319232363049,
0.996771768218699));
#15682=CARTESIAN_POINT('Ctrl Pts',(-0.364750145543744,-0.28018331644634,
1.01272583306292));
#15683=CARTESIAN_POINT('Ctrl Pts',(-0.340838910881557,-0.29104845371857,
1.02112815447116));
#15684=CARTESIAN_POINT('Ctrl Pts',(-0.290495481564827,-0.30527573347708,
1.036574285215));
#15685=CARTESIAN_POINT('Ctrl Pts',(-0.264056468041074,-0.308638795020976,
1.04359501395068));
#15686=CARTESIAN_POINT('Ctrl Pts',(-0.214892249704082,-0.308638795020976,
1.05481642595959));
#15687=CARTESIAN_POINT('Ctrl Pts',(-0.188025341585962,-0.30527573347708,
1.05996242598502));
#15688=CARTESIAN_POINT('Ctrl Pts',(-0.135965654106109,-0.29104845371857,
1.06788913840721));
#15689=CARTESIAN_POINT('Ctrl Pts',(-0.110776745452494,-0.28018331644634,
1.07069360430242));
#15690=CARTESIAN_POINT('Ctrl Pts',(-0.0663467128214646,-0.254319232363049,
1.07438230428002));
#15691=CARTESIAN_POINT('Ctrl Pts',(-0.0448960436540983,-0.237895043532788,
1.07542044338697));
#15692=CARTESIAN_POINT('Ctrl Pts',(-0.00674037211528124,-0.199697230012983,
1.07633607767727));
#15693=CARTESIAN_POINT('Ctrl Pts',(0.00996567398334777,-0.177924977804098,
1.07622728347683));
#15694=CARTESIAN_POINT('Ctrl Pts',(0.0404772621979741,-0.124911173756694,
1.07556023164702));
#15695=CARTESIAN_POINT('Ctrl Pts',(0.0525234025782719,-0.0925528133349865,
1.07492508698591));
#15696=CARTESIAN_POINT('Ctrl Pts',(0.0589974094846124,-0.05953,1.07456964270265));
#15697=CARTESIAN_POINT('Origin',(-0.244773027351946,-0.05953,1.07242070340001));
#15698=CARTESIAN_POINT('Origin',(0.,-0.05953,0.));
#15699=CARTESIAN_POINT('',(-0.803348093619616,-0.05953,0.716109245731214));
#15700=CARTESIAN_POINT('Origin',(0.,-0.05953,0.));
#15701=CARTESIAN_POINT('Origin',(-0.991065754692661,-0.05953,0.477272113029314));
#15702=CARTESIAN_POINT('Origin',(-0.991065754692661,0.,0.477272113029314));
#15703=CARTESIAN_POINT('',(-1.06075609691358,-0.05953,0.181596019242328));
#15704=CARTESIAN_POINT('Ctrl Pts',(-1.06075609691358,-0.05953,0.181596019242328));
#15705=CARTESIAN_POINT('Ctrl Pts',(-1.05966202740332,-0.0925528133349865,
0.187986803072856));
#15706=CARTESIAN_POINT('Ctrl Pts',(-1.05760072925372,-0.124911173756694,
0.199872254546857));
#15707=CARTESIAN_POINT('Ctrl Pts',(-1.05146158959546,-0.177924977804098,
0.22976728653846));
#15708=CARTESIAN_POINT('Ctrl Pts',(-1.04785021111757,-0.199697230012983,
0.246078686169301));
#15709=CARTESIAN_POINT('Ctrl Pts',(-1.03846709802406,-0.237895043532788,
0.283073967563097));
#15710=CARTESIAN_POINT('Ctrl Pts',(-1.03268176429485,-0.254319232363049,
0.303755815985685));
#15711=CARTESIAN_POINT('Ctrl Pts',(-1.01919893537026,-0.28018331644634,
0.346251081972725));
#15712=CARTESIAN_POINT('Ctrl Pts',(-1.01085972381132,-0.29104845371857,
0.370184399726282));
#15713=CARTESIAN_POINT('Ctrl Pts',(-0.99154738033959,-0.30527573347708,
0.419174982698463));
#15714=CARTESIAN_POINT('Ctrl Pts',(-0.980551951791748,-0.308638795020976,
0.444223188605045));
#15715=CARTESIAN_POINT('Ctrl Pts',(-0.958671816228589,-0.308638795020976,
0.489657758261848));
#15716=CARTESIAN_POINT('Ctrl Pts',(-0.945943877838127,-0.30527573347708,
0.51387163140139));
#15717=CARTESIAN_POINT('Ctrl Pts',(-0.91968254693063,-0.29104845371857,
0.559515758398093));
#15718=CARTESIAN_POINT('Ctrl Pts',(-0.906170138993533,-0.28018331644634,
0.580957796077825));
#15719=CARTESIAN_POINT('Ctrl Pts',(-0.8813524085237,-0.254319232363049,
0.617994461173994));
#15720=CARTESIAN_POINT('Ctrl Pts',(-0.868789784891799,-0.237895043532788,
0.635412538795143));
#15721=CARTESIAN_POINT('Ctrl Pts',(-0.845715984518854,-0.199697230012983,
0.66581473268113));
#15722=CARTESIAN_POINT('Ctrl Pts',(-0.835214876415962,-0.177924977804098,
0.678808213394124));
#15723=CARTESIAN_POINT('Ctrl Pts',(-0.815669690204649,-0.124911173756694,
0.702247233627224));
#15724=CARTESIAN_POINT('Ctrl Pts',(-0.807662468433796,-0.0925528133349865,
0.711269279199861));
#15725=CARTESIAN_POINT('Ctrl Pts',(-0.803348093619616,-0.05953,0.716109245731214));
#15726=CARTESIAN_POINT('Origin',(-0.991065754692661,-0.05953,0.477272113029314));
#15727=CARTESIAN_POINT('Origin',(0.,-0.05953,0.));
#15728=CARTESIAN_POINT('',(-1.076188,-0.05953,1.31795018948079E-16));
#15729=CARTESIAN_POINT('Origin',(0.,-0.05953,0.));
#15730=CARTESIAN_POINT('',(-1.06075609691358,-0.05953,-0.181596019242328));
#15731=CARTESIAN_POINT('Origin',(0.,-0.05953,0.));
#15732=CARTESIAN_POINT('Origin',(-0.991065754692661,-0.05953,-0.477272113029314));
#15733=CARTESIAN_POINT('Origin',(-0.991065754692661,0.,-0.477272113029314));
#15734=CARTESIAN_POINT('',(-0.803348093619616,-0.05953,-0.716109245731215));
#15735=CARTESIAN_POINT('Ctrl Pts',(-0.803348093619616,-0.05953,-0.716109245731215));
#15736=CARTESIAN_POINT('Ctrl Pts',(-0.807662468433795,-0.0925528133349865,
-0.711269279199862));
#15737=CARTESIAN_POINT('Ctrl Pts',(-0.815669690204649,-0.124911173756694,
-0.702247233627224));
#15738=CARTESIAN_POINT('Ctrl Pts',(-0.835214876415962,-0.177924977804098,
-0.678808213394124));
#15739=CARTESIAN_POINT('Ctrl Pts',(-0.845715984518854,-0.199697230012983,
-0.66581473268113));
#15740=CARTESIAN_POINT('Ctrl Pts',(-0.868789784891799,-0.237895043532788,
-0.635412538795143));
#15741=CARTESIAN_POINT('Ctrl Pts',(-0.8813524085237,-0.254319232363049,
-0.617994461173994));
#15742=CARTESIAN_POINT('Ctrl Pts',(-0.906170138993533,-0.28018331644634,
-0.580957796077826));
#15743=CARTESIAN_POINT('Ctrl Pts',(-0.91968254693063,-0.29104845371857,
-0.559515758398093));
#15744=CARTESIAN_POINT('Ctrl Pts',(-0.945943877838127,-0.30527573347708,
-0.51387163140139));
#15745=CARTESIAN_POINT('Ctrl Pts',(-0.958671816228589,-0.308638795020976,
-0.489657758261848));
#15746=CARTESIAN_POINT('Ctrl Pts',(-0.980551951791748,-0.308638795020976,
-0.444223188605045));
#15747=CARTESIAN_POINT('Ctrl Pts',(-0.99154738033959,-0.30527573347708,
-0.419174982698463));
#15748=CARTESIAN_POINT('Ctrl Pts',(-1.01085972381132,-0.29104845371857,
-0.370184399726282));
#15749=CARTESIAN_POINT('Ctrl Pts',(-1.01919893537026,-0.28018331644634,
-0.346251081972725));
#15750=CARTESIAN_POINT('Ctrl Pts',(-1.03268176429485,-0.254319232363049,
-0.303755815985685));
#15751=CARTESIAN_POINT('Ctrl Pts',(-1.03846709802406,-0.237895043532788,
-0.283073967563097));
#15752=CARTESIAN_POINT('Ctrl Pts',(-1.04785021111757,-0.199697230012983,
-0.246078686169302));
#15753=CARTESIAN_POINT('Ctrl Pts',(-1.05146158959546,-0.177924977804098,
-0.229767286538461));
#15754=CARTESIAN_POINT('Ctrl Pts',(-1.05760072925372,-0.124911173756694,
-0.199872254546858));
#15755=CARTESIAN_POINT('Ctrl Pts',(-1.05966202740332,-0.0925528133349864,
-0.187986803072857));
#15756=CARTESIAN_POINT('Ctrl Pts',(-1.06075609691358,-0.05953,-0.181596019242328));
#15757=CARTESIAN_POINT('Origin',(-0.991065754692661,-0.05953,-0.477272113029314));
#15758=CARTESIAN_POINT('Origin',(0.,-0.05953,0.));
#15759=CARTESIAN_POINT('',(-0.519393123750572,-0.05953,-0.942555777842682));
#15760=CARTESIAN_POINT('Origin',(0.,-0.05953,0.));
#15761=CARTESIAN_POINT('Origin',(-0.244773027351946,-0.05953,-1.07242070340001));
#15762=CARTESIAN_POINT('Origin',(-0.244773027351946,0.,-1.07242070340001));
#15763=CARTESIAN_POINT('',(0.0589974094846125,-0.05953,-1.07456964270265));
#15764=CARTESIAN_POINT('Ctrl Pts',(0.0589974094846127,-0.05953,-1.07456964270265));
#15765=CARTESIAN_POINT('Ctrl Pts',(0.0525234025782722,-0.0925528133349865,
-1.07492508698591));
#15766=CARTESIAN_POINT('Ctrl Pts',(0.0404772621979744,-0.124911173756694,
-1.07556023164702));
#15767=CARTESIAN_POINT('Ctrl Pts',(0.0099656739833481,-0.177924977804098,
-1.07622728347683));
#15768=CARTESIAN_POINT('Ctrl Pts',(-0.00674037211528096,-0.199697230012983,
-1.07633607767727));
#15769=CARTESIAN_POINT('Ctrl Pts',(-0.044896043654098,-0.237895043532788,
-1.07542044338697));
#15770=CARTESIAN_POINT('Ctrl Pts',(-0.0663467128214644,-0.254319232363049,
-1.07438230428002));
#15771=CARTESIAN_POINT('Ctrl Pts',(-0.110776745452493,-0.28018331644634,
-1.07069360430242));
#15772=CARTESIAN_POINT('Ctrl Pts',(-0.135965654106109,-0.29104845371857,
-1.06788913840721));
#15773=CARTESIAN_POINT('Ctrl Pts',(-0.188025341585962,-0.30527573347708,
-1.05996242598502));
#15774=CARTESIAN_POINT('Ctrl Pts',(-0.214892249704082,-0.308638795020976,
-1.05481642595959));
#15775=CARTESIAN_POINT('Ctrl Pts',(-0.264056468041074,-0.308638795020976,
-1.04359501395068));
#15776=CARTESIAN_POINT('Ctrl Pts',(-0.290495481564827,-0.30527573347708,
-1.036574285215));
#15777=CARTESIAN_POINT('Ctrl Pts',(-0.340838910881557,-0.291048453718569,
-1.02112815447116));
#15778=CARTESIAN_POINT('Ctrl Pts',(-0.364750145543744,-0.28018331644634,
-1.01272583306292));
#15779=CARTESIAN_POINT('Ctrl Pts',(-0.406380688682952,-0.254319232363049,
-0.996771768218699));
#15780=CARTESIAN_POINT('Ctrl Pts',(-0.426157505475872,-0.237895043532788,
-0.988400002689705));
#15781=CARTESIAN_POINT('Ctrl Pts',(-0.460931856495794,-0.199697230012983,
-0.972669835243841));
#15782=CARTESIAN_POINT('Ctrl Pts',(-0.475936279901919,-0.177924977804098,
-0.965323333309091));
#15783=CARTESIAN_POINT('Ctrl Pts',(-0.503136848051454,-0.124911173756694,
-0.951483858396181));
#15784=CARTESIAN_POINT('Ctrl Pts',(-0.513714466572041,-0.0925528133349865,
-0.945684988399766));
#15785=CARTESIAN_POINT('Ctrl Pts',(-0.519393123750572,-0.05953,-0.942555777842682));
#15786=CARTESIAN_POINT('Origin',(-0.244773027351946,-0.05953,-1.07242070340001));
#15787=CARTESIAN_POINT('Origin',(0.,-0.05953,0.));
#15788=CARTESIAN_POINT('',(0.413083465285518,-0.05953,-0.993751811093549));
#15789=CARTESIAN_POINT('Origin',(0.,-0.05953,0.));
#15790=CARTESIAN_POINT('Origin',(0.685838782044607,-0.05953,-0.860014630714833));
#15791=CARTESIAN_POINT('Origin',(0.685838782044607,0.,-0.860014630714833));
#15792=CARTESIAN_POINT('',(0.876916659919095,-0.05953,-0.623857181492959));
#15793=CARTESIAN_POINT('Ctrl Pts',(0.876916659919095,-0.05953,-0.623857181492958));
#15794=CARTESIAN_POINT('Ctrl Pts',(0.873158080166742,-0.0925528133349865,
-0.62914037979579));
#15795=CARTESIAN_POINT('Ctrl Pts',(0.866144010579847,-0.124911173756694,
-0.638954437806245));
#15796=CARTESIAN_POINT('Ctrl Pts',(0.847641868610495,-0.177924977804098,
-0.663225258065736));
#15797=CARTESIAN_POINT('Ctrl Pts',(0.837310877969633,-0.199697230012983,
-0.676354402927683));
#15798=CARTESIAN_POINT('Ctrl Pts',(0.81280533416753,-0.237895043532788,
-0.705614819529209));
#15799=CARTESIAN_POINT('Ctrl Pts',(0.798619410861634,-0.254319232363049,
-0.721738358858166));
#15800=CARTESIAN_POINT('Ctrl Pts',(0.768033796848072,-0.28018331644634,
-0.754175290318038));
#15801=CARTESIAN_POINT('Ctrl Pts',(0.750136149454208,-0.29104845371857,
-0.772120216227122));
#15802=CARTESIAN_POINT('Ctrl Pts',(0.711480111898423,-0.30527573347708,
-0.807879894508811));
#15803=CARTESIAN_POINT('Ctrl Pts',(0.690705563850638,-0.308638795020976,
-0.825676810575913));
#15804=CARTESIAN_POINT('Ctrl Pts',(0.651278921914856,-0.308638795020976,
-0.857118508332695));
#15805=CARTESIAN_POINT('Ctrl Pts',(0.629305439856167,-0.30527573347708,
-0.873412008702649));
#15806=CARTESIAN_POINT('Ctrl Pts',(0.585840553788742,-0.29104845371857,
-0.903141581680914));
#15807=CARTESIAN_POINT('Ctrl Pts',(0.564362943424239,-0.28018331644634,
-0.916597376014514));
#15808=CARTESIAN_POINT('Ctrl Pts',(0.525933334162556,-0.254319232363049,
-0.939198248544427));
#15809=CARTESIAN_POINT('Ctrl Pts',(0.507057380724533,-0.237895043532788,
-0.949440676105255));
#15810=CARTESIAN_POINT('Ctrl Pts',(0.473077587363686,-0.199697230012983,
-0.966820759530997));
#15811=CARTESIAN_POINT('Ctrl Pts',(0.457978755888596,-0.177924977804098,
-0.973971221090534));
#15812=CARTESIAN_POINT('Ctrl Pts',(0.430199341854858,-0.124911173756694,
-0.986608710139579));
#15813=CARTESIAN_POINT('Ctrl Pts',(0.419070565453384,-0.0925528133349865,
-0.991263089003441));
#15814=CARTESIAN_POINT('Ctrl Pts',(0.413083465285518,-0.05953,-0.993751811093549));
#15815=CARTESIAN_POINT('Origin',(0.685838782044607,-0.05953,-0.860014630714833));
#15816=CARTESIAN_POINT('Origin',(0.,-0.208355,0.));
#15817=CARTESIAN_POINT('',(-1.076188,-0.35718,1.31795018948079E-16));
#15818=CARTESIAN_POINT('Origin',(0.,-0.35718,0.));
#15819=CARTESIAN_POINT('',(-1.076188,-0.208355,1.31795018948079E-16));
#15820=CARTESIAN_POINT('',(1.03449977959455,-0.05953,0.296632461748266));
#15821=CARTESIAN_POINT('Origin',(0.,-0.05953,0.));
#15822=CARTESIAN_POINT('',(1.03449977959455,-0.05953,-0.296632461748266));
#15823=CARTESIAN_POINT('Ctrl Pts',(1.03449977959455,-0.05953,0.296632461748267));
#15824=CARTESIAN_POINT('Ctrl Pts',(1.03628691421076,-0.0925528133349865,
0.290399865505497));
#15825=CARTESIAN_POINT('Ctrl Pts',(1.03958665287714,-0.124911173756694,
0.278797079997872));
#15826=CARTESIAN_POINT('Ctrl Pts',(1.0470264474309,-0.177924977804098,0.249198913998601));
#15827=CARTESIAN_POINT('Ctrl Pts',(1.05084995891418,-0.199697230012983,
0.232935932341942));
#15828=CARTESIAN_POINT('Ctrl Pts',(1.05844771715377,-0.237895043532788,
0.195533155353269));
#15829=CARTESIAN_POINT('Ctrl Pts',(1.06220882929878,-0.254319232363049,
0.17438929156337));
#15830=CARTESIAN_POINT('Ctrl Pts',(1.06849922508772,-0.28018331644634,0.130252399648131));
#15831=CARTESIAN_POINT('Ctrl Pts',(1.07137013248666,-0.29104845371857,0.105070977154072));
#15832=CARTESIAN_POINT('Ctrl Pts',(1.07522652957392,-0.30527573347708,0.0525526752791107));
#15833=CARTESIAN_POINT('Ctrl Pts',(1.076188,-0.308638795020976,0.025214283908933));
#15834=CARTESIAN_POINT('Ctrl Pts',(1.076188,-0.308638795020976,-0.025214283908933));
#15835=CARTESIAN_POINT('Ctrl Pts',(1.07522652957392,-0.30527573347708,-0.0525526752791107));
#15836=CARTESIAN_POINT('Ctrl Pts',(1.07137013248666,-0.29104845371857,-0.105070977154072));
#15837=CARTESIAN_POINT('Ctrl Pts',(1.06849922508772,-0.28018331644634,-0.130252399648131));
#15838=CARTESIAN_POINT('Ctrl Pts',(1.06220882929878,-0.254319232363049,
-0.17438929156337));
#15839=CARTESIAN_POINT('Ctrl Pts',(1.05844771715377,-0.237895043532788,
-0.195533155353269));
#15840=CARTESIAN_POINT('Ctrl Pts',(1.05084995891418,-0.199697230012983,
-0.232935932341942));
#15841=CARTESIAN_POINT('Ctrl Pts',(1.0470264474309,-0.177924977804098,-0.249198913998601));
#15842=CARTESIAN_POINT('Ctrl Pts',(1.03958665287714,-0.124911173756694,
-0.278797079997872));
#15843=CARTESIAN_POINT('Ctrl Pts',(1.03628691421076,-0.0925528133349865,
-0.290399865505497));
#15844=CARTESIAN_POINT('Ctrl Pts',(1.03449977959455,-0.05953,-0.296632461748267));
#15845=CARTESIAN_POINT('Origin',(0.,-0.05953,0.));
#15846=CARTESIAN_POINT('Origin',(0.,-0.05953,0.));
#15847=CARTESIAN_POINT('Origin',(1.1,-0.05953,0.));
#15848=CARTESIAN_POINT('Origin',(1.1,0.,0.));
#15849=CARTESIAN_POINT('Origin',(1.1,-0.05953,0.));
#15850=CARTESIAN_POINT('Origin',(0.,-0.35718,0.));
#15851=CARTESIAN_POINT('Origin',(0.,-0.05953,0.));
#15852=CARTESIAN_POINT('',(0.,0.,0.));
#15853=CARTESIAN_POINT('Origin',(1.119765,0.495,0.));
#15854=CARTESIAN_POINT('',(-1.119765,0.495,-1.37131662304724E-16));
#15855=CARTESIAN_POINT('Origin',(0.,0.495,0.));
#15856=CARTESIAN_POINT('',(-1.085235,0.495,-1.32902956907268E-16));
#15857=CARTESIAN_POINT('Origin',(0.,0.495,0.));
#15858=CARTESIAN_POINT('Origin',(0.,0.4575,0.));
#15859=CARTESIAN_POINT('',(-1.119765,0.42,-1.37131662304724E-16));
#15860=CARTESIAN_POINT('Origin',(0.,0.42,0.));
#15861=CARTESIAN_POINT('',(-1.119765,0.4575,-1.37131662304724E-16));
#15862=CARTESIAN_POINT('Origin',(1.085235,0.42,0.));
#15863=CARTESIAN_POINT('',(-1.085235,0.42,-1.32902956907268E-16));
#15864=CARTESIAN_POINT('Origin',(0.,0.42,0.));
#15865=CARTESIAN_POINT('Origin',(0.,0.4575,0.));
#15866=CARTESIAN_POINT('',(-1.085235,0.4575,-1.32902956907268E-16));
#15867=CARTESIAN_POINT('Origin',(1.119765,-0.42,0.));
#15868=CARTESIAN_POINT('',(-1.119765,-0.42,-1.37131662304724E-16));
#15869=CARTESIAN_POINT('Origin',(0.,-0.42,0.));
#15870=CARTESIAN_POINT('',(-1.085235,-0.42,-1.32902956907268E-16));
#15871=CARTESIAN_POINT('Origin',(0.,-0.42,0.));
#15872=CARTESIAN_POINT('Origin',(0.,-0.4575,0.));
#15873=CARTESIAN_POINT('',(-1.119765,-0.495,-1.37131662304724E-16));
#15874=CARTESIAN_POINT('Origin',(0.,-0.495,0.));
#15875=CARTESIAN_POINT('',(-1.119765,-0.4575,-1.37131662304724E-16));
#15876=CARTESIAN_POINT('Origin',(1.085235,-0.495,0.));
#15877=CARTESIAN_POINT('',(-1.085235,-0.495,-1.32902956907268E-16));
#15878=CARTESIAN_POINT('Origin',(0.,-0.495,0.));
#15879=CARTESIAN_POINT('Origin',(0.,-0.4575,0.));
#15880=CARTESIAN_POINT('',(-1.085235,-0.4575,-1.32902956907268E-16));
#15881=CARTESIAN_POINT('',(0.,0.,0.));
#15882=CARTESIAN_POINT('',(0.,0.,0.));
#15883=CARTESIAN_POINT('',(0.,0.,0.));
#15884=CARTESIAN_POINT('',(0.,0.,0.));
#15885=CARTESIAN_POINT('',(0.,0.,0.));
#15886=CARTESIAN_POINT('',(0.,0.,0.));
#15887=CARTESIAN_POINT('Origin',(0.0866025403784439,-0.4,-0.15));
#15888=CARTESIAN_POINT('',(0.173205080756888,-0.4,0.));
#15889=CARTESIAN_POINT('',(0.0866025403784439,-0.4,-0.15));
#15890=CARTESIAN_POINT('',(0.173205080756888,-0.4,0.));
#15891=CARTESIAN_POINT('',(0.0866025403784439,-0.64,-0.15));
#15892=CARTESIAN_POINT('',(0.0866025403784439,-0.4,-0.15));
#15893=CARTESIAN_POINT('',(0.173205080756888,-0.64,0.));
#15894=CARTESIAN_POINT('',(0.173205080756888,-0.64,0.));
#15895=CARTESIAN_POINT('',(0.173205080756888,-0.4,0.));
#15896=CARTESIAN_POINT('Origin',(-0.0866025403784438,-0.4,-0.15));
#15897=CARTESIAN_POINT('',(-0.0866025403784438,-0.4,-0.15));
#15898=CARTESIAN_POINT('',(0.0866025403784439,-0.4,-0.15));
#15899=CARTESIAN_POINT('',(-0.0866025403784438,-0.64,-0.15));
#15900=CARTESIAN_POINT('',(-0.0866025403784438,-0.4,-0.15));
#15901=CARTESIAN_POINT('',(0.0866025403784439,-0.64,-0.15));
#15902=CARTESIAN_POINT('Origin',(-0.173205080756888,-0.4,-2.77555756156289E-17));
#15903=CARTESIAN_POINT('',(-0.173205080756888,-0.4,-2.12115047744981E-17));
#15904=CARTESIAN_POINT('',(-0.0866025403784438,-0.4,-0.15));
#15905=CARTESIAN_POINT('',(-0.173205080756888,-0.64,-2.77555756156289E-17));
#15906=CARTESIAN_POINT('',(-0.173205080756888,-0.4,-2.12115047744981E-17));
#15907=CARTESIAN_POINT('',(-0.0866025403784438,-0.64,-0.15));
#15908=CARTESIAN_POINT('Origin',(-0.0866025403784439,-0.4,0.15));
#15909=CARTESIAN_POINT('',(-0.0866025403784439,-0.4,0.15));
#15910=CARTESIAN_POINT('',(-0.173205080756888,-0.4,-2.12115047744981E-17));
#15911=CARTESIAN_POINT('',(-0.0866025403784439,-0.64,0.15));
#15912=CARTESIAN_POINT('',(-0.0866025403784439,-0.4,0.15));
#15913=CARTESIAN_POINT('',(-0.173205080756888,-0.64,-2.12115047744981E-17));
#15914=CARTESIAN_POINT('Origin',(0.0866025403784439,-0.4,0.15));
#15915=CARTESIAN_POINT('',(0.0866025403784439,-0.4,0.15));
#15916=CARTESIAN_POINT('',(-0.0866025403784439,-0.4,0.15));
#15917=CARTESIAN_POINT('',(0.0866025403784439,-0.64,0.15));
#15918=CARTESIAN_POINT('',(0.0866025403784439,-0.4,0.15));
#15919=CARTESIAN_POINT('',(-0.0866025403784439,-0.64,0.15));
#15920=CARTESIAN_POINT('Origin',(0.173205080756888,-0.4,0.));
#15921=CARTESIAN_POINT('',(0.0866025403784439,-0.4,0.15));
#15922=CARTESIAN_POINT('',(0.0866025403784439,-0.64,0.15));
#15923=CARTESIAN_POINT('Origin',(0.,-0.4,-2.77555756156289E-17));
#15924=CARTESIAN_POINT('Origin',(0.,-0.64,-2.77555756156289E-17));
#15925=CARTESIAN_POINT('Origin',(0.,-1.,0.));
#15926=CARTESIAN_POINT('',(-0.1954,-1.,2.39295984553393E-17));
#15927=CARTESIAN_POINT('Origin',(0.,-1.,0.));
#15928=CARTESIAN_POINT('Origin',(0.3,0.4,0.));
#15929=CARTESIAN_POINT('',(-0.3,0.4,-3.67394039744206E-17));
#15930=CARTESIAN_POINT('Origin',(0.,0.4,0.));
#15931=CARTESIAN_POINT('Origin',(0.,0.375,0.));
#15932=CARTESIAN_POINT('',(-0.35,0.35,-4.28626379701573E-17));
#15933=CARTESIAN_POINT('Origin',(0.,0.35,0.));
#15934=CARTESIAN_POINT('',(-0.325,0.375,-3.9801020972289E-17));
#15935=CARTESIAN_POINT('Origin',(0.,0.19,0.));
#15936=CARTESIAN_POINT('',(-0.35,0.03,-4.28626379701574E-17));
#15937=CARTESIAN_POINT('Origin',(0.,0.03,0.));
#15938=CARTESIAN_POINT('',(-0.35,0.19,-4.28626379701574E-17));
#15939=CARTESIAN_POINT('Origin',(0.,0.0149999999999999,0.));
#15940=CARTESIAN_POINT('',(-0.32,-3.29597460435593E-17,-3.91886975727153E-17));
#15941=CARTESIAN_POINT('Origin',(0.,0.,0.));
#15942=CARTESIAN_POINT('',(-0.335,0.0149999999999999,-4.10256677714363E-17));
#15943=CARTESIAN_POINT('Origin',(0.22,0.,0.));
#15944=CARTESIAN_POINT('',(-0.22,-6.93889390390723E-18,-2.69422295812418E-17));
#15945=CARTESIAN_POINT('Origin',(0.,0.,0.));
#15946=CARTESIAN_POINT('Origin',(0.,-0.02,0.));
#15947=CARTESIAN_POINT('',(-0.1954,-0.0492,2.39295984553393E-17));
#15948=CARTESIAN_POINT('Origin',(0.,-0.0492,0.));
#15949=CARTESIAN_POINT('',(-0.21,-0.02,-2.57175827820944E-17));
#15950=CARTESIAN_POINT('Origin',(0.,-0.8,0.));
#15951=CARTESIAN_POINT('',(-0.1954,-0.8,-2.39295984553393E-17));
#15952=CARTESIAN_POINT('',(0.,0.,0.));
#15953=CARTESIAN_POINT('',(0.,0.,0.));
#15954=CARTESIAN_POINT('Origin',(0.,-5.1,7.));
#15955=CARTESIAN_POINT('',(-0.165,-5.,7.));
#15956=CARTESIAN_POINT('Origin',(0.,-5.,7.));
#15957=CARTESIAN_POINT('',(-0.165,-3.4,7.));
#15958=CARTESIAN_POINT('',(-0.165,-5.1,7.));
#15959=CARTESIAN_POINT('Origin',(0.,-3.4,7.));
#15960=CARTESIAN_POINT('Origin',(0.,-3.4,7.));
#15961=CARTESIAN_POINT('Origin',(0.,2.05,7.));
#15962=CARTESIAN_POINT('',(-0.7,2.05,7.));
#15963=CARTESIAN_POINT('Origin',(0.,2.05,7.));
#15964=CARTESIAN_POINT('',(-0.5,2.05,7.));
#15965=CARTESIAN_POINT('Origin',(0.,2.05,7.));
#15966=CARTESIAN_POINT('Origin',(0.,1.35,7.));
#15967=CARTESIAN_POINT('',(-0.7,1.35,7.));
#15968=CARTESIAN_POINT('Origin',(0.,1.35,7.));
#15969=CARTESIAN_POINT('',(-0.5,1.35,7.));
#15970=CARTESIAN_POINT('Origin',(0.,1.35,7.));
#15971=CARTESIAN_POINT('Origin',(0.,1.35,7.));
#15972=CARTESIAN_POINT('',(-0.7,1.35,7.));
#15973=CARTESIAN_POINT('Origin',(0.,-1.8,7.));
#15974=CARTESIAN_POINT('',(-0.5,-1.8,7.));
#15975=CARTESIAN_POINT('',(-0.5,-1.8,7.));
#15976=CARTESIAN_POINT('Origin',(0.,-1.8,7.));
#15977=CARTESIAN_POINT('Origin',(0.,-5.,7.));
#15978=CARTESIAN_POINT('',(-0.4,-1.8,7.));
#15979=CARTESIAN_POINT('Origin',(0.,-1.8,7.));
#15980=CARTESIAN_POINT('',(-0.4,-5.,7.));
#15981=CARTESIAN_POINT('',(-0.4,-5.,7.));
#15982=CARTESIAN_POINT('Origin',(0.,-5.,7.));
#15983=CARTESIAN_POINT('Origin',(0.,-5.,7.));
#15984=CARTESIAN_POINT('Origin',(0.,-1.8,7.));
#15985=CARTESIAN_POINT('',(-0.5,3.,7.));
#15986=CARTESIAN_POINT('Origin',(0.,3.,7.));
#15987=CARTESIAN_POINT('',(-0.5,-1.8,7.));
#15988=CARTESIAN_POINT('Origin',(0.,3.,7.));
#15989=CARTESIAN_POINT('Origin',(0.,-1.8,7.));
#15990=CARTESIAN_POINT('',(0.,0.,0.));
#15991=CARTESIAN_POINT('Origin',(0.,-1.8,7.));
#15992=CARTESIAN_POINT('',(-0.505,-1.8,7.));
#15993=CARTESIAN_POINT('Origin',(0.,-1.8,7.));
#15994=CARTESIAN_POINT('',(-0.505,-1.35,7.));
#15995=CARTESIAN_POINT('',(-0.505,-1.8,7.));
#15996=CARTESIAN_POINT('Origin',(0.,-1.35,7.));
#15997=CARTESIAN_POINT('Origin',(0.,-1.8,7.));
#15998=CARTESIAN_POINT('',(-0.405,-1.8,7.));
#15999=CARTESIAN_POINT('Origin',(0.,-1.8,7.));
#16000=CARTESIAN_POINT('Origin',(0.,-2.65,7.));
#16001=CARTESIAN_POINT('',(-0.405,-2.65,7.));
#16002=CARTESIAN_POINT('',(-0.405,-2.65,7.));
#16003=CARTESIAN_POINT('Origin',(0.,-2.65,7.));
#16004=CARTESIAN_POINT('Origin',(0.,-2.65,7.));
#16005=CARTESIAN_POINT('',(-0.7,-1.35,7.));
#16006=CARTESIAN_POINT('Origin',(0.,-1.35,7.));
#16007=CARTESIAN_POINT('',(-0.7,-2.65,7.));
#16008=CARTESIAN_POINT('',(-0.7,-2.65,7.));
#16009=CARTESIAN_POINT('Origin',(0.,-2.65,7.));
#16010=CARTESIAN_POINT('Origin',(0.,-1.35,7.));
#16011=CARTESIAN_POINT('Origin',(0.,-2.65,7.));
#16012=CARTESIAN_POINT('',(0.,0.,0.));
#16013=CARTESIAN_POINT('Origin',(0.,-0.45,7.));
#16014=CARTESIAN_POINT('',(-0.505,0.45,7.));
#16015=CARTESIAN_POINT('Origin',(0.,0.45,7.));
#16016=CARTESIAN_POINT('',(-0.505,-0.45,7.));
#16017=CARTESIAN_POINT('',(-0.505,-0.45,7.));
#16018=CARTESIAN_POINT('Origin',(0.,-0.45,7.));
#16019=CARTESIAN_POINT('Origin',(0.,-0.45,7.));
#16020=CARTESIAN_POINT('',(-0.7,0.45,7.));
#16021=CARTESIAN_POINT('Origin',(0.,0.45,7.));
#16022=CARTESIAN_POINT('',(-0.7,-0.45,7.));
#16023=CARTESIAN_POINT('',(-0.7,-0.45,7.));
#16024=CARTESIAN_POINT('Origin',(0.,-0.45,7.));
#16025=CARTESIAN_POINT('Origin',(0.,0.45,7.));
#16026=CARTESIAN_POINT('Origin',(0.,-0.45,7.));
#16027=CARTESIAN_POINT('',(0.,0.,0.));
#16028=CARTESIAN_POINT('Origin',(0.,-3.95,6.35));
#16029=CARTESIAN_POINT('',(-0.15,-3.95,6.6));
#16030=CARTESIAN_POINT('Origin',(0.,-3.95,6.6));
#16031=CARTESIAN_POINT('',(-0.15,-3.95,6.35));
#16032=CARTESIAN_POINT('',(-0.15,-3.95,6.35));
#16033=CARTESIAN_POINT('Origin',(0.,-3.95,6.35));
#16034=CARTESIAN_POINT('Origin',(0.,-3.95,6.6));
#16035=CARTESIAN_POINT('Origin',(0.,-3.95,6.35));
#16036=CARTESIAN_POINT('',(0.,0.,0.));
#16037=CARTESIAN_POINT('Origin',(0.,-3.95,7.4));
#16038=CARTESIAN_POINT('',(-0.15,-3.95,7.65));
#16039=CARTESIAN_POINT('Origin',(0.,-3.95,7.65));
#16040=CARTESIAN_POINT('',(-0.15,-3.95,7.4));
#16041=CARTESIAN_POINT('',(-0.15,-3.95,7.4));
#16042=CARTESIAN_POINT('Origin',(0.,-3.95,7.4));
#16043=CARTESIAN_POINT('Origin',(0.,-3.95,7.65));
#16044=CARTESIAN_POINT('Origin',(0.,-3.95,7.4));
#16045=CARTESIAN_POINT('',(0.,0.,0.));
#16046=CARTESIAN_POINT('Origin',(0.,-5.2,7.));
#16047=CARTESIAN_POINT('',(-0.225,-5.,7.));
#16048=CARTESIAN_POINT('Origin',(0.,-5.,7.));
#16049=CARTESIAN_POINT('',(-0.225,-5.2,7.));
#16050=CARTESIAN_POINT('',(-0.225,-5.2,7.));
#16051=CARTESIAN_POINT('Origin',(0.,-5.2,7.));
#16052=CARTESIAN_POINT('Origin',(0.,-5.2,7.));
#16053=CARTESIAN_POINT('',(-0.6,-5.,7.));
#16054=CARTESIAN_POINT('Origin',(0.,-5.,7.));
#16055=CARTESIAN_POINT('',(-0.6,-5.2,7.));
#16056=CARTESIAN_POINT('',(-0.6,-5.2,7.));
#16057=CARTESIAN_POINT('Origin',(0.,-5.2,7.));
#16058=CARTESIAN_POINT('Origin',(0.,-5.,7.));
#16059=CARTESIAN_POINT('Origin',(0.,-5.2,7.));
#16060=CARTESIAN_POINT('',(0.,0.,0.));
#16061=CARTESIAN_POINT('Origin',(0.,-0.45,0.));
#16062=CARTESIAN_POINT('',(-0.65,-0.325,-3.9801020972289E-17));
#16063=CARTESIAN_POINT('',(-0.637867541108654,-0.45,0.125));
#16064=CARTESIAN_POINT('Ctrl Pts',(-0.65,-0.325,-6.93889390390723E-17));
#16065=CARTESIAN_POINT('Ctrl Pts',(-0.65,-0.325,0.0157371373481997));
#16066=CARTESIAN_POINT('Ctrl Pts',(-0.649370620646074,-0.328153081062251,
0.0324967135411163));
#16067=CARTESIAN_POINT('Ctrl Pts',(-0.647096224417991,-0.340922081922822,
0.0632828231545122));
#16068=CARTESIAN_POINT('Ctrl Pts',(-0.645482573914132,-0.350535859112198,
0.0773125544088347));
#16069=CARTESIAN_POINT('Ctrl Pts',(-0.642442040715078,-0.372687974598127,
0.0994646698947638));
#16070=CARTESIAN_POINT('Ctrl Pts',(-0.640815160902589,-0.386717480603274,
0.109078032552995));
#16071=CARTESIAN_POINT('Ctrl Pts',(-0.63851034608138,-0.417502809542363,
0.121846732641678));
#16072=CARTESIAN_POINT('Ctrl Pts',(-0.637867541108654,-0.434262111007648,
0.125));
#16073=CARTESIAN_POINT('Ctrl Pts',(-0.637867541108654,-0.45,0.125));
#16074=CARTESIAN_POINT('',(-0.65,-0.575,-3.9801020972289E-17));
#16075=CARTESIAN_POINT('Ctrl Pts',(-0.65,-0.575,-3.46944695195361E-18));
#16076=CARTESIAN_POINT('Ctrl Pts',(-0.65,-0.575,-0.0157371373481998));
#16077=CARTESIAN_POINT('Ctrl Pts',(-0.649370620646074,-0.571846918937749,
-0.0324967135411164));
#16078=CARTESIAN_POINT('Ctrl Pts',(-0.647096224417991,-0.559077918077178,
-0.0632828231545123));
#16079=CARTESIAN_POINT('Ctrl Pts',(-0.645482573914132,-0.549464140887802,
-0.0773125544088349));
#16080=CARTESIAN_POINT('Ctrl Pts',(-0.642442040715078,-0.527312025401873,
-0.099464669894764));
#16081=CARTESIAN_POINT('Ctrl Pts',(-0.640815160902589,-0.513282519396725,
-0.109078032552995));
#16082=CARTESIAN_POINT('Ctrl Pts',(-0.63851034608138,-0.482497190457637,
-0.121846732641678));
#16083=CARTESIAN_POINT('Ctrl Pts',(-0.637867541108654,-0.465737888992352,
-0.125));
#16084=CARTESIAN_POINT('Ctrl Pts',(-0.637867541108654,-0.434262111007648,
-0.125));
#16085=CARTESIAN_POINT('Ctrl Pts',(-0.63851034608138,-0.417502809542363,
-0.121846732641678));
#16086=CARTESIAN_POINT('Ctrl Pts',(-0.640815160902589,-0.386717480603275,
-0.109078032552995));
#16087=CARTESIAN_POINT('Ctrl Pts',(-0.642442040715078,-0.372687974598127,
-0.099464669894764));
#16088=CARTESIAN_POINT('Ctrl Pts',(-0.645482573914132,-0.350535859112198,
-0.077312554408835));
#16089=CARTESIAN_POINT('Ctrl Pts',(-0.647096224417991,-0.340922081922822,
-0.0632828231545124));
#16090=CARTESIAN_POINT('Ctrl Pts',(-0.649370620646074,-0.328153081062251,
-0.0324967135411165));
#16091=CARTESIAN_POINT('Ctrl Pts',(-0.65,-0.325,-0.0157371373481999));
#16092=CARTESIAN_POINT('Ctrl Pts',(-0.65,-0.325,-8.32667268468867E-17));
#16093=CARTESIAN_POINT('Ctrl Pts',(-0.637867541108654,-0.45,0.125));
#16094=CARTESIAN_POINT('Ctrl Pts',(-0.637867541108654,-0.465737888992352,
0.125));
#16095=CARTESIAN_POINT('Ctrl Pts',(-0.63851034608138,-0.482497190457637,
0.121846732641678));
#16096=CARTESIAN_POINT('Ctrl Pts',(-0.640815160902589,-0.513282519396725,
0.109078032552995));
#16097=CARTESIAN_POINT('Ctrl Pts',(-0.642442040715078,-0.527312025401873,
0.0994646698947639));
#16098=CARTESIAN_POINT('Ctrl Pts',(-0.645482573914132,-0.549464140887802,
0.0773125544088349));
#16099=CARTESIAN_POINT('Ctrl Pts',(-0.647096224417991,-0.559077918077178,
0.0632828231545123));
#16100=CARTESIAN_POINT('Ctrl Pts',(-0.649370620646074,-0.571846918937749,
0.0324967135411164));
#16101=CARTESIAN_POINT('Ctrl Pts',(-0.65,-0.575,0.0157371373481998));
#16102=CARTESIAN_POINT('Ctrl Pts',(-0.65,-0.575,-2.08166817117217E-17));
#16103=CARTESIAN_POINT('',(-0.379967103839267,-0.45,0.125));
#16104=CARTESIAN_POINT('',(-7.65404249467096E-18,-0.45,0.125));
#16105=CARTESIAN_POINT('',(-0.4,-0.575,5.41097774720219E-18));
#16106=CARTESIAN_POINT('Ctrl Pts',(-0.4,-0.575,-3.81639164714898E-17));
#16107=CARTESIAN_POINT('Ctrl Pts',(-0.4,-0.575,0.0158075115832675));
#16108=CARTESIAN_POINT('Ctrl Pts',(-0.398970551469948,-0.571819306519379,
0.0325978607437828));
#16109=CARTESIAN_POINT('Ctrl Pts',(-0.395252954914593,-0.559029081159106,
0.0633657881355917));
#16110=CARTESIAN_POINT('Ctrl Pts',(-0.392612801026882,-0.549425200318011,
0.0773514949786256));
#16111=CARTESIAN_POINT('Ctrl Pts',(-0.38761064154154,-0.527347592689753,
0.0994291026068839));
#16112=CARTESIAN_POINT('Ctrl Pts',(-0.384911758361269,-0.51336346023721,
0.109029967924066));
#16113=CARTESIAN_POINT('Ctrl Pts',(-0.381057715344782,-0.48260129709332,
0.121817958968287));
#16114=CARTESIAN_POINT('Ctrl Pts',(-0.379967103839267,-0.465813100629203,
0.125));
#16115=CARTESIAN_POINT('Ctrl Pts',(-0.379967103839267,-0.45,0.125));
#16116=CARTESIAN_POINT('',(-0.379967103839267,-0.45,-0.125));
#16117=CARTESIAN_POINT('Ctrl Pts',(-0.379967103839267,-0.45,-0.125));
#16118=CARTESIAN_POINT('Ctrl Pts',(-0.379967103839267,-0.465813100629203,
-0.125));
#16119=CARTESIAN_POINT('Ctrl Pts',(-0.381057715344782,-0.48260129709332,
-0.121817958968287));
#16120=CARTESIAN_POINT('Ctrl Pts',(-0.384911758361269,-0.51336346023721,
-0.109029967924066));
#16121=CARTESIAN_POINT('Ctrl Pts',(-0.38761064154154,-0.527347592689753,
-0.099429102606884));
#16122=CARTESIAN_POINT('Ctrl Pts',(-0.392612801026882,-0.549425200318011,
-0.0773514949786257));
#16123=CARTESIAN_POINT('Ctrl Pts',(-0.395252954914593,-0.559029081159106,
-0.0633657881355918));
#16124=CARTESIAN_POINT('Ctrl Pts',(-0.398970551469948,-0.571819306519379,
-0.0325978607437828));
#16125=CARTESIAN_POINT('Ctrl Pts',(-0.4,-0.575,-0.0158075115832676));
#16126=CARTESIAN_POINT('Ctrl Pts',(-0.4,-0.575,-4.16333634234434E-17));
#16127=CARTESIAN_POINT('',(-0.4,-0.325,2.96971064108775E-17));
#16128=CARTESIAN_POINT('Ctrl Pts',(-0.4,-0.325,1.04083408558608E-17));
#16129=CARTESIAN_POINT('Ctrl Pts',(-0.4,-0.325,-0.0158075115832676));
#16130=CARTESIAN_POINT('Ctrl Pts',(-0.398970551469948,-0.328180693480621,
-0.0325978607437828));
#16131=CARTESIAN_POINT('Ctrl Pts',(-0.395252954914593,-0.340970918840894,
-0.0633657881355918));
#16132=CARTESIAN_POINT('Ctrl Pts',(-0.392612801026882,-0.350574799681989,
-0.0773514949786256));
#16133=CARTESIAN_POINT('Ctrl Pts',(-0.38761064154154,-0.372652407310247,
-0.0994291026068839));
#16134=CARTESIAN_POINT('Ctrl Pts',(-0.384911758361269,-0.38663653976279,
-0.109029967924066));
#16135=CARTESIAN_POINT('Ctrl Pts',(-0.381057715344782,-0.41739870290668,
-0.121817958968287));
#16136=CARTESIAN_POINT('Ctrl Pts',(-0.379967103839267,-0.434186899370797,
-0.125));
#16137=CARTESIAN_POINT('Ctrl Pts',(-0.379967103839267,-0.45,-0.125));
#16138=CARTESIAN_POINT('Ctrl Pts',(-0.379967103839267,-0.45,0.125));
#16139=CARTESIAN_POINT('Ctrl Pts',(-0.379967103839267,-0.434186899370797,
0.125));
#16140=CARTESIAN_POINT('Ctrl Pts',(-0.381057715344782,-0.41739870290668,
0.121817958968287));
#16141=CARTESIAN_POINT('Ctrl Pts',(-0.384911758361269,-0.38663653976279,
0.109029967924066));
#16142=CARTESIAN_POINT('Ctrl Pts',(-0.38761064154154,-0.372652407310247,
0.0994291026068839));
#16143=CARTESIAN_POINT('Ctrl Pts',(-0.392612801026882,-0.350574799681989,
0.0773514949786257));
#16144=CARTESIAN_POINT('Ctrl Pts',(-0.395252954914593,-0.340970918840894,
0.0633657881355918));
#16145=CARTESIAN_POINT('Ctrl Pts',(-0.398970551469948,-0.328180693480621,
0.0325978607437829));
#16146=CARTESIAN_POINT('Ctrl Pts',(-0.4,-0.325,0.0158075115832676));
#16147=CARTESIAN_POINT('Ctrl Pts',(-0.4,-0.325,1.38777878078145E-17));
#16148=CARTESIAN_POINT('Origin',(0.,-0.45,0.));
#16149=CARTESIAN_POINT('',(0.379967103839267,-0.45,-0.125));
#16150=CARTESIAN_POINT('',(0.379967103839267,-0.45,0.125));
#16151=CARTESIAN_POINT('Ctrl Pts',(0.379967103839267,-0.45,-0.125));
#16152=CARTESIAN_POINT('Ctrl Pts',(0.379967103839267,-0.434186899370797,
-0.125));
#16153=CARTESIAN_POINT('Ctrl Pts',(0.381057715344782,-0.41739870290668,
-0.121817958968287));
#16154=CARTESIAN_POINT('Ctrl Pts',(0.384911758361269,-0.38663653976279,
-0.109029967924066));
#16155=CARTESIAN_POINT('Ctrl Pts',(0.38761064154154,-0.372652407310247,
-0.0994291026068839));
#16156=CARTESIAN_POINT('Ctrl Pts',(0.392612801026882,-0.350574799681989,
-0.0773514949786256));
#16157=CARTESIAN_POINT('Ctrl Pts',(0.395252954914593,-0.340970918840894,
-0.0633657881355917));
#16158=CARTESIAN_POINT('Ctrl Pts',(0.398970551469948,-0.328180693480621,
-0.0325978607437828));
#16159=CARTESIAN_POINT('Ctrl Pts',(0.4,-0.325,-0.0158075115832675));
#16160=CARTESIAN_POINT('Ctrl Pts',(0.4,-0.325,0.0158075115832676));
#16161=CARTESIAN_POINT('Ctrl Pts',(0.398970551469948,-0.328180693480621,
0.0325978607437829));
#16162=CARTESIAN_POINT('Ctrl Pts',(0.395252954914593,-0.340970918840894,
0.0633657881355918));
#16163=CARTESIAN_POINT('Ctrl Pts',(0.392612801026882,-0.350574799681989,
0.0773514949786257));
#16164=CARTESIAN_POINT('Ctrl Pts',(0.38761064154154,-0.372652407310247,
0.099429102606884));
#16165=CARTESIAN_POINT('Ctrl Pts',(0.384911758361269,-0.38663653976279,
0.109029967924066));
#16166=CARTESIAN_POINT('Ctrl Pts',(0.381057715344782,-0.41739870290668,
0.121817958968287));
#16167=CARTESIAN_POINT('Ctrl Pts',(0.379967103839267,-0.434186899370797,
0.125));
#16168=CARTESIAN_POINT('Ctrl Pts',(0.379967103839267,-0.45,0.125));
#16169=CARTESIAN_POINT('Ctrl Pts',(0.379967103839267,-0.45,0.125));
#16170=CARTESIAN_POINT('Ctrl Pts',(0.379967103839267,-0.465813100629203,
0.125));
#16171=CARTESIAN_POINT('Ctrl Pts',(0.381057715344782,-0.48260129709332,
0.121817958968287));
#16172=CARTESIAN_POINT('Ctrl Pts',(0.384911758361269,-0.51336346023721,
0.109029967924066));
#16173=CARTESIAN_POINT('Ctrl Pts',(0.38761064154154,-0.527347592689753,
0.0994291026068839));
#16174=CARTESIAN_POINT('Ctrl Pts',(0.392612801026882,-0.549425200318011,
0.0773514949786257));
#16175=CARTESIAN_POINT('Ctrl Pts',(0.395252954914593,-0.559029081159106,
0.0633657881355918));
#16176=CARTESIAN_POINT('Ctrl Pts',(0.398970551469948,-0.571819306519379,
0.0325978607437829));
#16177=CARTESIAN_POINT('Ctrl Pts',(0.4,-0.575,0.0158075115832676));
#16178=CARTESIAN_POINT('Ctrl Pts',(0.4,-0.575,-0.0158075115832676));
#16179=CARTESIAN_POINT('Ctrl Pts',(0.398970551469948,-0.57181930651938,
-0.0325978607437828));
#16180=CARTESIAN_POINT('Ctrl Pts',(0.395252954914593,-0.559029081159106,
-0.0633657881355918));
#16181=CARTESIAN_POINT('Ctrl Pts',(0.392612801026882,-0.549425200318011,
-0.0773514949786257));
#16182=CARTESIAN_POINT('Ctrl Pts',(0.38761064154154,-0.527347592689753,
-0.0994291026068839));
#16183=CARTESIAN_POINT('Ctrl Pts',(0.384911758361269,-0.51336346023721,
-0.109029967924066));
#16184=CARTESIAN_POINT('Ctrl Pts',(0.381057715344782,-0.48260129709332,
-0.121817958968287));
#16185=CARTESIAN_POINT('Ctrl Pts',(0.379967103839267,-0.465813100629203,
-0.125));
#16186=CARTESIAN_POINT('Ctrl Pts',(0.379967103839267,-0.45,-0.125));
#16187=CARTESIAN_POINT('',(0.637867541108654,-0.45,0.125));
#16188=CARTESIAN_POINT('',(-7.65404249467096E-18,-0.45,0.125));
#16189=CARTESIAN_POINT('',(0.65,-0.575,3.9801020972289E-17));
#16190=CARTESIAN_POINT('Ctrl Pts',(0.65,-0.575,5.55111512312578E-17));
#16191=CARTESIAN_POINT('Ctrl Pts',(0.65,-0.575,0.0157371373481999));
#16192=CARTESIAN_POINT('Ctrl Pts',(0.649370620646074,-0.571846918937749,
0.0324967135411165));
#16193=CARTESIAN_POINT('Ctrl Pts',(0.647096224417991,-0.559077918077178,
0.0632828231545124));
#16194=CARTESIAN_POINT('Ctrl Pts',(0.645482573914132,-0.549464140887802,
0.077312554408835));
#16195=CARTESIAN_POINT('Ctrl Pts',(0.642442040715078,-0.527312025401873,
0.099464669894764));
#16196=CARTESIAN_POINT('Ctrl Pts',(0.640815160902589,-0.513282519396725,
0.109078032552995));
#16197=CARTESIAN_POINT('Ctrl Pts',(0.63851034608138,-0.482497190457637,
0.121846732641678));
#16198=CARTESIAN_POINT('Ctrl Pts',(0.637867541108654,-0.465737888992352,
0.125));
#16199=CARTESIAN_POINT('Ctrl Pts',(0.637867541108654,-0.45,0.125));
#16200=CARTESIAN_POINT('',(0.65,-0.325,3.9801020972289E-17));
#16201=CARTESIAN_POINT('Ctrl Pts',(0.65,-0.325,6.93889390390723E-18));
#16202=CARTESIAN_POINT('Ctrl Pts',(0.65,-0.325,-0.0157371373481998));
#16203=CARTESIAN_POINT('Ctrl Pts',(0.649370620646074,-0.328153081062251,
-0.0324967135411164));
#16204=CARTESIAN_POINT('Ctrl Pts',(0.647096224417991,-0.340922081922822,
-0.0632828231545123));
#16205=CARTESIAN_POINT('Ctrl Pts',(0.645482573914132,-0.350535859112198,
-0.0773125544088349));
#16206=CARTESIAN_POINT('Ctrl Pts',(0.642442040715078,-0.372687974598127,
-0.0994646698947639));
#16207=CARTESIAN_POINT('Ctrl Pts',(0.640815160902588,-0.386717480603275,
-0.109078032552995));
#16208=CARTESIAN_POINT('Ctrl Pts',(0.63851034608138,-0.417502809542363,
-0.121846732641678));
#16209=CARTESIAN_POINT('Ctrl Pts',(0.637867541108654,-0.434262111007648,
-0.125));
#16210=CARTESIAN_POINT('Ctrl Pts',(0.637867541108654,-0.465737888992352,
-0.125));
#16211=CARTESIAN_POINT('Ctrl Pts',(0.63851034608138,-0.482497190457637,
-0.121846732641678));
#16212=CARTESIAN_POINT('Ctrl Pts',(0.640815160902589,-0.513282519396725,
-0.109078032552995));
#16213=CARTESIAN_POINT('Ctrl Pts',(0.642442040715078,-0.527312025401873,
-0.0994646698947639));
#16214=CARTESIAN_POINT('Ctrl Pts',(0.645482573914132,-0.549464140887802,
-0.0773125544088348));
#16215=CARTESIAN_POINT('Ctrl Pts',(0.647096224417991,-0.559077918077178,
-0.0632828231545123));
#16216=CARTESIAN_POINT('Ctrl Pts',(0.649370620646074,-0.571846918937749,
-0.0324967135411164));
#16217=CARTESIAN_POINT('Ctrl Pts',(0.65,-0.575,-0.0157371373481998));
#16218=CARTESIAN_POINT('Ctrl Pts',(0.65,-0.575,6.24500451351651E-17));
#16219=CARTESIAN_POINT('Ctrl Pts',(0.637867541108654,-0.45,0.125));
#16220=CARTESIAN_POINT('Ctrl Pts',(0.637867541108654,-0.434262111007648,
0.125));
#16221=CARTESIAN_POINT('Ctrl Pts',(0.63851034608138,-0.417502809542363,
0.121846732641678));
#16222=CARTESIAN_POINT('Ctrl Pts',(0.640815160902589,-0.386717480603274,
0.109078032552995));
#16223=CARTESIAN_POINT('Ctrl Pts',(0.642442040715078,-0.372687974598127,
0.0994646698947639));
#16224=CARTESIAN_POINT('Ctrl Pts',(0.645482573914132,-0.350535859112198,
0.0773125544088348));
#16225=CARTESIAN_POINT('Ctrl Pts',(0.647096224417991,-0.340922081922822,
0.0632828231545123));
#16226=CARTESIAN_POINT('Ctrl Pts',(0.649370620646074,-0.328153081062251,
0.0324967135411164));
#16227=CARTESIAN_POINT('Ctrl Pts',(0.65,-0.325,0.0157371373481998));
#16228=CARTESIAN_POINT('Ctrl Pts',(0.65,-0.325,-6.93889390390723E-18));
#16229=CARTESIAN_POINT('Origin',(0.,-0.1,0.));
#16230=CARTESIAN_POINT('',(-0.65,-0.8,7.9602041944578E-17));
#16231=CARTESIAN_POINT('Origin',(0.,-0.8,0.));
#16232=CARTESIAN_POINT('',(-0.65,-0.1,-7.9602041944578E-17));
#16233=CARTESIAN_POINT('',(-0.65,-0.1,7.9602041944578E-17));
#16234=CARTESIAN_POINT('',(-0.65,-0.1,-7.9602041944578E-17));
#16235=CARTESIAN_POINT('Origin',(0.,-0.1,0.));
#16236=CARTESIAN_POINT('',(0.,-0.575,-0.65));
#16237=CARTESIAN_POINT('',(0.,-0.325,-0.65));
#16238=CARTESIAN_POINT('Ctrl Pts',(-1.73472347597681E-17,-0.575,-0.65));
#16239=CARTESIAN_POINT('Ctrl Pts',(0.0157371373481998,-0.575,-0.65));
#16240=CARTESIAN_POINT('Ctrl Pts',(0.0324967135411164,-0.571846918937749,
-0.649370620646074));
#16241=CARTESIAN_POINT('Ctrl Pts',(0.0632828231545123,-0.559077918077178,
-0.647096224417991));
#16242=CARTESIAN_POINT('Ctrl Pts',(0.0773125544088349,-0.549464140887802,
-0.645482573914132));
#16243=CARTESIAN_POINT('Ctrl Pts',(0.099464669894764,-0.527312025401873,
-0.642442040715078));
#16244=CARTESIAN_POINT('Ctrl Pts',(0.109078032552995,-0.513282519396725,
-0.640815160902589));
#16245=CARTESIAN_POINT('Ctrl Pts',(0.121846732641678,-0.482497190457636,
-0.63851034608138));
#16246=CARTESIAN_POINT('Ctrl Pts',(0.125,-0.465737888992352,-0.637867541108654));
#16247=CARTESIAN_POINT('Ctrl Pts',(0.125,-0.434262111007648,-0.637867541108654));
#16248=CARTESIAN_POINT('Ctrl Pts',(0.121846732641678,-0.417502809542364,
-0.63851034608138));
#16249=CARTESIAN_POINT('Ctrl Pts',(0.109078032552995,-0.386717480603275,
-0.640815160902589));
#16250=CARTESIAN_POINT('Ctrl Pts',(0.099464669894764,-0.372687974598127,
-0.642442040715078));
#16251=CARTESIAN_POINT('Ctrl Pts',(0.0773125544088349,-0.350535859112198,
-0.645482573914132));
#16252=CARTESIAN_POINT('Ctrl Pts',(0.0632828231545123,-0.340922081922822,
-0.647096224417991));
#16253=CARTESIAN_POINT('Ctrl Pts',(0.0324967135411164,-0.328153081062251,
-0.649370620646074));
#16254=CARTESIAN_POINT('Ctrl Pts',(0.0157371373481999,-0.325,-0.65));
#16255=CARTESIAN_POINT('Ctrl Pts',(4.5102810375397E-17,-0.325,-0.65));
#16256=CARTESIAN_POINT('',(-0.125,-0.45,-0.637867541108654));
#16257=CARTESIAN_POINT('Ctrl Pts',(4.85722573273506E-17,-0.325,-0.65));
#16258=CARTESIAN_POINT('Ctrl Pts',(-0.0157371373481997,-0.325,-0.65));
#16259=CARTESIAN_POINT('Ctrl Pts',(-0.0324967135411163,-0.328153081062251,
-0.649370620646074));
#16260=CARTESIAN_POINT('Ctrl Pts',(-0.0632828231545122,-0.340922081922822,
-0.647096224417991));
#16261=CARTESIAN_POINT('Ctrl Pts',(-0.0773125544088348,-0.350535859112198,
-0.645482573914132));
#16262=CARTESIAN_POINT('Ctrl Pts',(-0.0994646698947639,-0.372687974598127,
-0.642442040715078));
#16263=CARTESIAN_POINT('Ctrl Pts',(-0.109078032552995,-0.386717480603274,
-0.640815160902589));
#16264=CARTESIAN_POINT('Ctrl Pts',(-0.121846732641678,-0.417502809542363,
-0.63851034608138));
#16265=CARTESIAN_POINT('Ctrl Pts',(-0.125,-0.434262111007648,-0.637867541108654));
#16266=CARTESIAN_POINT('Ctrl Pts',(-0.125,-0.45,-0.637867541108654));
#16267=CARTESIAN_POINT('Ctrl Pts',(-0.125,-0.45,-0.637867541108654));
#16268=CARTESIAN_POINT('Ctrl Pts',(-0.125,-0.465737888992352,-0.637867541108654));
#16269=CARTESIAN_POINT('Ctrl Pts',(-0.121846732641678,-0.482497190457636,
-0.63851034608138));
#16270=CARTESIAN_POINT('Ctrl Pts',(-0.109078032552995,-0.513282519396725,
-0.640815160902589));
#16271=CARTESIAN_POINT('Ctrl Pts',(-0.099464669894764,-0.527312025401873,
-0.642442040715078));
#16272=CARTESIAN_POINT('Ctrl Pts',(-0.0773125544088349,-0.549464140887802,
-0.645482573914132));
#16273=CARTESIAN_POINT('Ctrl Pts',(-0.0632828231545124,-0.559077918077178,
-0.647096224417991));
#16274=CARTESIAN_POINT('Ctrl Pts',(-0.0324967135411165,-0.571846918937749,
-0.649370620646074));
#16275=CARTESIAN_POINT('Ctrl Pts',(-0.0157371373481998,-0.575,-0.65));
#16276=CARTESIAN_POINT('Ctrl Pts',(-1.73472347597681E-17,-0.575,-0.65));
#16277=CARTESIAN_POINT('',(0.,-0.325,0.65));
#16278=CARTESIAN_POINT('',(0.,-0.575,0.65));
#16279=CARTESIAN_POINT('Ctrl Pts',(2.77555756156289E-17,-0.325,0.65));
#16280=CARTESIAN_POINT('Ctrl Pts',(0.0157371373481998,-0.325,0.65));
#16281=CARTESIAN_POINT('Ctrl Pts',(0.0324967135411164,-0.328153081062251,
0.649370620646074));
#16282=CARTESIAN_POINT('Ctrl Pts',(0.0632828231545123,-0.340922081922822,
0.647096224417991));
#16283=CARTESIAN_POINT('Ctrl Pts',(0.0773125544088349,-0.350535859112198,
0.645482573914132));
#16284=CARTESIAN_POINT('Ctrl Pts',(0.099464669894764,-0.372687974598127,
0.642442040715078));
#16285=CARTESIAN_POINT('Ctrl Pts',(0.109078032552995,-0.386717480603275,
0.640815160902589));
#16286=CARTESIAN_POINT('Ctrl Pts',(0.121846732641678,-0.417502809542364,
0.63851034608138));
#16287=CARTESIAN_POINT('Ctrl Pts',(0.125,-0.434262111007648,0.637867541108654));
#16288=CARTESIAN_POINT('Ctrl Pts',(0.125,-0.465737888992352,0.637867541108654));
#16289=CARTESIAN_POINT('Ctrl Pts',(0.121846732641678,-0.482497190457636,
0.63851034608138));
#16290=CARTESIAN_POINT('Ctrl Pts',(0.109078032552995,-0.513282519396725,
0.640815160902589));
#16291=CARTESIAN_POINT('Ctrl Pts',(0.099464669894764,-0.527312025401873,
0.642442040715078));
#16292=CARTESIAN_POINT('Ctrl Pts',(0.077312554408835,-0.549464140887802,
0.645482573914132));
#16293=CARTESIAN_POINT('Ctrl Pts',(0.0632828231545124,-0.559077918077178,
0.647096224417991));
#16294=CARTESIAN_POINT('Ctrl Pts',(0.0324967135411165,-0.571846918937749,
0.649370620646074));
#16295=CARTESIAN_POINT('Ctrl Pts',(0.0157371373481998,-0.575,0.65));
#16296=CARTESIAN_POINT('Ctrl Pts',(-1.38777878078145E-17,-0.575,0.65));
#16297=CARTESIAN_POINT('',(-0.125,-0.45,0.637867541108654));
#16298=CARTESIAN_POINT('Ctrl Pts',(-1.04083408558608E-17,-0.575,0.65));
#16299=CARTESIAN_POINT('Ctrl Pts',(-0.0157371373481998,-0.575,0.65));
#16300=CARTESIAN_POINT('Ctrl Pts',(-0.0324967135411164,-0.571846918937749,
0.649370620646074));
#16301=CARTESIAN_POINT('Ctrl Pts',(-0.0632828231545123,-0.559077918077178,
0.647096224417991));
#16302=CARTESIAN_POINT('Ctrl Pts',(-0.0773125544088349,-0.549464140887802,
0.645482573914132));
#16303=CARTESIAN_POINT('Ctrl Pts',(-0.099464669894764,-0.527312025401873,
0.642442040715078));
#16304=CARTESIAN_POINT('Ctrl Pts',(-0.109078032552995,-0.513282519396725,
0.640815160902589));
#16305=CARTESIAN_POINT('Ctrl Pts',(-0.121846732641678,-0.482497190457636,
0.63851034608138));
#16306=CARTESIAN_POINT('Ctrl Pts',(-0.125,-0.465737888992352,0.637867541108654));
#16307=CARTESIAN_POINT('Ctrl Pts',(-0.125,-0.45,0.637867541108654));
#16308=CARTESIAN_POINT('Ctrl Pts',(-0.125,-0.45,0.637867541108654));
#16309=CARTESIAN_POINT('Ctrl Pts',(-0.125,-0.434262111007648,0.637867541108654));
#16310=CARTESIAN_POINT('Ctrl Pts',(-0.121846732641678,-0.417502809542363,
0.63851034608138));
#16311=CARTESIAN_POINT('Ctrl Pts',(-0.109078032552995,-0.386717480603274,
0.640815160902589));
#16312=CARTESIAN_POINT('Ctrl Pts',(-0.0994646698947639,-0.372687974598127,
0.642442040715078));
#16313=CARTESIAN_POINT('Ctrl Pts',(-0.0773125544088348,-0.350535859112198,
0.645482573914132));
#16314=CARTESIAN_POINT('Ctrl Pts',(-0.0632828231545122,-0.340922081922822,
0.647096224417991));
#16315=CARTESIAN_POINT('Ctrl Pts',(-0.0324967135411163,-0.328153081062251,
0.649370620646074));
#16316=CARTESIAN_POINT('Ctrl Pts',(-0.0157371373481998,-0.325,0.65));
#16317=CARTESIAN_POINT('Ctrl Pts',(4.5102810375397E-17,-0.325,0.65));
#16318=CARTESIAN_POINT('Origin',(0.,-0.45,0.));
#16319=CARTESIAN_POINT('',(-0.125,-0.45,-0.379967103839267));
#16320=CARTESIAN_POINT('',(-0.125,-0.45,0.));
#16321=CARTESIAN_POINT('',(0.125,-0.45,-0.379967103839267));
#16322=CARTESIAN_POINT('Ctrl Pts',(0.125,-0.45,-0.379967103839267));
#16323=CARTESIAN_POINT('Ctrl Pts',(0.125,-0.465813100629203,-0.379967103839267));
#16324=CARTESIAN_POINT('Ctrl Pts',(0.121817958968287,-0.48260129709332,
-0.381057715344782));
#16325=CARTESIAN_POINT('Ctrl Pts',(0.109029967924066,-0.51336346023721,
-0.384911758361269));
#16326=CARTESIAN_POINT('Ctrl Pts',(0.0994291026068839,-0.527347592689753,
-0.38761064154154));
#16327=CARTESIAN_POINT('Ctrl Pts',(0.0773514949786257,-0.549425200318011,
-0.392612801026882));
#16328=CARTESIAN_POINT('Ctrl Pts',(0.0633657881355918,-0.559029081159106,
-0.395252954914593));
#16329=CARTESIAN_POINT('Ctrl Pts',(0.0325978607437828,-0.571819306519379,
-0.398970551469948));
#16330=CARTESIAN_POINT('Ctrl Pts',(0.0158075115832676,-0.575,-0.4));
#16331=CARTESIAN_POINT('Ctrl Pts',(-0.0158075115832676,-0.575,-0.4));
#16332=CARTESIAN_POINT('Ctrl Pts',(-0.0325978607437828,-0.571819306519379,
-0.398970551469948));
#16333=CARTESIAN_POINT('Ctrl Pts',(-0.0633657881355918,-0.559029081159106,
-0.395252954914593));
#16334=CARTESIAN_POINT('Ctrl Pts',(-0.0773514949786256,-0.549425200318011,
-0.392612801026882));
#16335=CARTESIAN_POINT('Ctrl Pts',(-0.0994291026068839,-0.527347592689753,
-0.38761064154154));
#16336=CARTESIAN_POINT('Ctrl Pts',(-0.109029967924066,-0.51336346023721,
-0.384911758361269));
#16337=CARTESIAN_POINT('Ctrl Pts',(-0.121817958968287,-0.48260129709332,
-0.381057715344782));
#16338=CARTESIAN_POINT('Ctrl Pts',(-0.125,-0.465813100629203,-0.379967103839267));
#16339=CARTESIAN_POINT('Ctrl Pts',(-0.125,-0.45,-0.379967103839267));
#16340=CARTESIAN_POINT('Ctrl Pts',(-0.125,-0.45,-0.379967103839267));
#16341=CARTESIAN_POINT('Ctrl Pts',(-0.125,-0.434186899370797,-0.379967103839267));
#16342=CARTESIAN_POINT('Ctrl Pts',(-0.121817958968287,-0.41739870290668,
-0.381057715344782));
#16343=CARTESIAN_POINT('Ctrl Pts',(-0.109029967924066,-0.38663653976279,
-0.384911758361269));
#16344=CARTESIAN_POINT('Ctrl Pts',(-0.0994291026068839,-0.372652407310247,
-0.38761064154154));
#16345=CARTESIAN_POINT('Ctrl Pts',(-0.0773514949786257,-0.350574799681989,
-0.392612801026882));
#16346=CARTESIAN_POINT('Ctrl Pts',(-0.0633657881355918,-0.340970918840894,
-0.395252954914593));
#16347=CARTESIAN_POINT('Ctrl Pts',(-0.0325978607437829,-0.328180693480621,
-0.398970551469948));
#16348=CARTESIAN_POINT('Ctrl Pts',(-0.0158075115832676,-0.325,-0.4));
#16349=CARTESIAN_POINT('Ctrl Pts',(0.0158075115832675,-0.325,-0.4));
#16350=CARTESIAN_POINT('Ctrl Pts',(0.0325978607437828,-0.328180693480621,
-0.398970551469948));
#16351=CARTESIAN_POINT('Ctrl Pts',(0.0633657881355917,-0.340970918840894,
-0.395252954914593));
#16352=CARTESIAN_POINT('Ctrl Pts',(0.0773514949786256,-0.350574799681989,
-0.392612801026882));
#16353=CARTESIAN_POINT('Ctrl Pts',(0.0994291026068839,-0.372652407310247,
-0.38761064154154));
#16354=CARTESIAN_POINT('Ctrl Pts',(0.109029967924066,-0.38663653976279,
-0.384911758361269));
#16355=CARTESIAN_POINT('Ctrl Pts',(0.121817958968287,-0.41739870290668,
-0.381057715344782));
#16356=CARTESIAN_POINT('Ctrl Pts',(0.125,-0.434186899370797,-0.379967103839267));
#16357=CARTESIAN_POINT('Ctrl Pts',(0.125,-0.45,-0.379967103839267));
#16358=CARTESIAN_POINT('Origin',(0.,-0.45,0.));
#16359=CARTESIAN_POINT('',(0.125,-0.45,0.379967103839267));
#16360=CARTESIAN_POINT('',(-0.125,-0.45,0.379967103839267));
#16361=CARTESIAN_POINT('Ctrl Pts',(0.125,-0.45,0.379967103839267));
#16362=CARTESIAN_POINT('Ctrl Pts',(0.125,-0.434186899370797,0.379967103839267));
#16363=CARTESIAN_POINT('Ctrl Pts',(0.121817958968287,-0.41739870290668,
0.381057715344782));
#16364=CARTESIAN_POINT('Ctrl Pts',(0.109029967924066,-0.38663653976279,
0.384911758361269));
#16365=CARTESIAN_POINT('Ctrl Pts',(0.0994291026068839,-0.372652407310247,
0.38761064154154));
#16366=CARTESIAN_POINT('Ctrl Pts',(0.0773514949786256,-0.350574799681989,
0.392612801026882));
#16367=CARTESIAN_POINT('Ctrl Pts',(0.0633657881355918,-0.340970918840894,
0.395252954914593));
#16368=CARTESIAN_POINT('Ctrl Pts',(0.0325978607437828,-0.328180693480621,
0.398970551469948));
#16369=CARTESIAN_POINT('Ctrl Pts',(0.0158075115832676,-0.325,0.4));
#16370=CARTESIAN_POINT('Ctrl Pts',(-0.0158075115832676,-0.325,0.4));
#16371=CARTESIAN_POINT('Ctrl Pts',(-0.0325978607437828,-0.328180693480621,
0.398970551469948));
#16372=CARTESIAN_POINT('Ctrl Pts',(-0.0633657881355918,-0.340970918840894,
0.395252954914593));
#16373=CARTESIAN_POINT('Ctrl Pts',(-0.0773514949786257,-0.350574799681989,
0.392612801026882));
#16374=CARTESIAN_POINT('Ctrl Pts',(-0.0994291026068839,-0.372652407310247,
0.38761064154154));
#16375=CARTESIAN_POINT('Ctrl Pts',(-0.109029967924066,-0.38663653976279,
0.384911758361269));
#16376=CARTESIAN_POINT('Ctrl Pts',(-0.121817958968287,-0.41739870290668,
0.381057715344782));
#16377=CARTESIAN_POINT('Ctrl Pts',(-0.125,-0.434186899370797,0.379967103839267));
#16378=CARTESIAN_POINT('Ctrl Pts',(-0.125,-0.45,0.379967103839267));
#16379=CARTESIAN_POINT('Ctrl Pts',(-0.125,-0.45,0.379967103839267));
#16380=CARTESIAN_POINT('Ctrl Pts',(-0.125,-0.465813100629203,0.379967103839267));
#16381=CARTESIAN_POINT('Ctrl Pts',(-0.121817958968287,-0.48260129709332,
0.381057715344782));
#16382=CARTESIAN_POINT('Ctrl Pts',(-0.109029967924066,-0.51336346023721,
0.384911758361269));
#16383=CARTESIAN_POINT('Ctrl Pts',(-0.0994291026068839,-0.527347592689753,
0.38761064154154));
#16384=CARTESIAN_POINT('Ctrl Pts',(-0.0773514949786256,-0.549425200318011,
0.392612801026882));
#16385=CARTESIAN_POINT('Ctrl Pts',(-0.0633657881355917,-0.559029081159106,
0.395252954914593));
#16386=CARTESIAN_POINT('Ctrl Pts',(-0.0325978607437828,-0.571819306519379,
0.398970551469948));
#16387=CARTESIAN_POINT('Ctrl Pts',(-0.0158075115832675,-0.575,0.4));
#16388=CARTESIAN_POINT('Ctrl Pts',(0.0158075115832676,-0.575,0.4));
#16389=CARTESIAN_POINT('Ctrl Pts',(0.0325978607437828,-0.571819306519379,
0.398970551469948));
#16390=CARTESIAN_POINT('Ctrl Pts',(0.0633657881355917,-0.559029081159106,
0.395252954914593));
#16391=CARTESIAN_POINT('Ctrl Pts',(0.0773514949786257,-0.549425200318011,
0.392612801026882));
#16392=CARTESIAN_POINT('Ctrl Pts',(0.0994291026068839,-0.527347592689753,
0.38761064154154));
#16393=CARTESIAN_POINT('Ctrl Pts',(0.109029967924066,-0.51336346023721,
0.384911758361269));
#16394=CARTESIAN_POINT('Ctrl Pts',(0.121817958968287,-0.48260129709332,
0.381057715344782));
#16395=CARTESIAN_POINT('Ctrl Pts',(0.125,-0.465813100629203,0.379967103839267));
#16396=CARTESIAN_POINT('Ctrl Pts',(0.125,-0.45,0.379967103839267));
#16397=CARTESIAN_POINT('',(-0.125,-0.45,0.));
#16398=CARTESIAN_POINT('Origin',(0.,0.,0.));
#16399=CARTESIAN_POINT('',(-0.4,-0.8,4.89858719658941E-17));
#16400=CARTESIAN_POINT('Origin',(0.,-0.8,0.));
#16401=CARTESIAN_POINT('',(-0.4,0.,4.89858719658941E-17));
#16402=CARTESIAN_POINT('',(-0.4,0.85,-4.89858719658941E-17));
#16403=CARTESIAN_POINT('',(-0.4,0.,4.89858719658941E-17));
#16404=CARTESIAN_POINT('Origin',(0.,0.85,0.));
#16405=CARTESIAN_POINT('Origin',(0.,-0.8,0.));
#16406=CARTESIAN_POINT('Origin',(0.,0.,0.));
#16407=CARTESIAN_POINT('',(-0.8,0.,9.79717439317883E-17));
#16408=CARTESIAN_POINT('Origin',(0.,0.,0.));
#16409=CARTESIAN_POINT('',(0.595438916863769,0.,0.137993139022126));
#16410=CARTESIAN_POINT('',(0.562830534889751,0.,0.238351419397483));
#16411=CARTESIAN_POINT('Origin',(0.562758945330873,0.,0.182851465569258));
#16412=CARTESIAN_POINT('',(0.523653836874034,0.,0.315240018494132));
#16413=CARTESIAN_POINT('Origin',(0.,0.,0.));
#16414=CARTESIAN_POINT('',(0.461629008549572,0.,0.40060987082025));
#16415=CARTESIAN_POINT('Origin',(0.478711351753049,0.,0.347804155687524));
#16416=CARTESIAN_POINT('',(0.40060987082025,0.,0.461629008549572));
#16417=CARTESIAN_POINT('Origin',(0.,0.,0.));
#16418=CARTESIAN_POINT('',(0.315240018494132,0.,0.523653836874034));
#16419=CARTESIAN_POINT('Origin',(0.347804155687523,0.,0.478711351753049));
#16420=CARTESIAN_POINT('',(0.238351419397483,0.,0.562830534889751));
#16421=CARTESIAN_POINT('Origin',(0.,0.,0.));
#16422=CARTESIAN_POINT('',(0.137993139022126,0.,0.595438916863769));
#16423=CARTESIAN_POINT('Origin',(0.182851465569258,0.,0.562758945330873));
#16424=CARTESIAN_POINT('',(0.0527614703521001,0.,0.608938287003997));
#16425=CARTESIAN_POINT('Origin',(0.,0.,0.));
#16426=CARTESIAN_POINT('',(-0.0527614703521003,0.,0.608938287003997));
#16427=CARTESIAN_POINT('Origin',(-1.08697158783324E-16,0.,0.591719772367581));
#16428=CARTESIAN_POINT('',(-0.137993139022126,0.,0.595438916863769));
#16429=CARTESIAN_POINT('Origin',(0.,0.,0.));
#16430=CARTESIAN_POINT('',(-0.238351419397483,0.,0.562830534889751));
#16431=CARTESIAN_POINT('Origin',(-0.182851465569258,0.,0.562758945330873));
#16432=CARTESIAN_POINT('',(-0.315240018494132,0.,0.523653836874034));
#16433=CARTESIAN_POINT('Origin',(0.,0.,0.));
#16434=CARTESIAN_POINT('',(-0.40060987082025,0.,0.461629008549572));
#16435=CARTESIAN_POINT('Origin',(-0.347804155687524,0.,0.478711351753049));
#16436=CARTESIAN_POINT('',(-0.461629008549572,0.,0.40060987082025));
#16437=CARTESIAN_POINT('Origin',(0.,0.,0.));
#16438=CARTESIAN_POINT('',(-0.523653836874034,0.,0.315240018494132));
#16439=CARTESIAN_POINT('Origin',(-0.478711351753049,0.,0.347804155687524));
#16440=CARTESIAN_POINT('',(-0.562830534889751,0.,0.238351419397483));
#16441=CARTESIAN_POINT('Origin',(0.,0.,0.));
#16442=CARTESIAN_POINT('',(-0.595438916863769,0.,0.137993139022126));
#16443=CARTESIAN_POINT('Origin',(-0.562758945330873,0.,0.182851465569258));
#16444=CARTESIAN_POINT('',(-0.608938287003997,0.,0.0527614703521002));
#16445=CARTESIAN_POINT('Origin',(0.,0.,0.));
#16446=CARTESIAN_POINT('',(-0.608938287003997,0.,-0.0527614703521003));
#16447=CARTESIAN_POINT('Origin',(-0.591719772367581,0.,-7.24647725222159E-17));
#16448=CARTESIAN_POINT('',(-0.595438916863769,0.,-0.137993139022126));
#16449=CARTESIAN_POINT('Origin',(0.,0.,0.));
#16450=CARTESIAN_POINT('',(-0.562830534889751,0.,-0.238351419397483));
#16451=CARTESIAN_POINT('Origin',(-0.562758945330873,0.,-0.182851465569258));
#16452=CARTESIAN_POINT('',(-0.523653836874034,0.,-0.315240018494132));
#16453=CARTESIAN_POINT('Origin',(0.,0.,0.));
#16454=CARTESIAN_POINT('',(-0.461629008549572,0.,-0.40060987082025));
#16455=CARTESIAN_POINT('Origin',(-0.478711351753049,0.,-0.347804155687524));
#16456=CARTESIAN_POINT('',(-0.40060987082025,0.,-0.461629008549572));
#16457=CARTESIAN_POINT('Origin',(0.,0.,0.));
#16458=CARTESIAN_POINT('',(-0.315240018494132,0.,-0.523653836874034));
#16459=CARTESIAN_POINT('Origin',(-0.347804155687524,0.,-0.478711351753049));
#16460=CARTESIAN_POINT('',(-0.238351419397483,0.,-0.562830534889751));
#16461=CARTESIAN_POINT('Origin',(0.,0.,0.));
#16462=CARTESIAN_POINT('',(-0.137993139022126,0.,-0.595438916863769));
#16463=CARTESIAN_POINT('Origin',(-0.182851465569258,0.,-0.562758945330873));
#16464=CARTESIAN_POINT('',(-0.0527614703521002,0.,-0.608938287003997));
#16465=CARTESIAN_POINT('Origin',(0.,0.,0.));
#16466=CARTESIAN_POINT('',(0.0527614703521003,0.,-0.608938287003997));
#16467=CARTESIAN_POINT('Origin',(3.6232386261108E-17,0.,-0.591719772367581));
#16468=CARTESIAN_POINT('',(0.137993139022126,0.,-0.595438916863769));
#16469=CARTESIAN_POINT('Origin',(0.,0.,0.));
#16470=CARTESIAN_POINT('',(0.238351419397483,0.,-0.562830534889751));
#16471=CARTESIAN_POINT('Origin',(0.182851465569258,0.,-0.562758945330873));
#16472=CARTESIAN_POINT('',(0.315240018494132,0.,-0.523653836874034));
#16473=CARTESIAN_POINT('Origin',(0.,0.,0.));
#16474=CARTESIAN_POINT('',(0.40060987082025,0.,-0.461629008549572));
#16475=CARTESIAN_POINT('Origin',(0.347804155687524,0.,-0.478711351753049));
#16476=CARTESIAN_POINT('',(0.461629008549572,0.,-0.40060987082025));
#16477=CARTESIAN_POINT('Origin',(0.,0.,0.));
#16478=CARTESIAN_POINT('',(0.523653836874034,0.,-0.315240018494132));
#16479=CARTESIAN_POINT('Origin',(0.478711351753049,0.,-0.347804155687524));
#16480=CARTESIAN_POINT('',(0.562830534889751,0.,-0.238351419397483));
#16481=CARTESIAN_POINT('Origin',(0.,0.,0.));
#16482=CARTESIAN_POINT('',(0.595438916863769,0.,-0.137993139022126));
#16483=CARTESIAN_POINT('Origin',(0.562758945330873,0.,-0.182851465569258));
#16484=CARTESIAN_POINT('',(0.608938287003997,0.,-0.0527614703521001));
#16485=CARTESIAN_POINT('Origin',(0.,0.,0.));
#16486=CARTESIAN_POINT('',(0.608938287003997,0.,0.0527614703521001));
#16487=CARTESIAN_POINT('Origin',(0.591719772367581,0.,0.));
#16488=CARTESIAN_POINT('Origin',(0.,0.,0.));
#16489=CARTESIAN_POINT('Origin',(0.,0.,0.));
#16490=CARTESIAN_POINT('',(-0.8,-0.1,9.79717439317883E-17));
#16491=CARTESIAN_POINT('Origin',(0.,-0.1,0.));
#16492=CARTESIAN_POINT('',(-0.8,0.,-9.79717439317883E-17));
#16493=CARTESIAN_POINT('Origin',(0.,-0.1,0.));
#16494=CARTESIAN_POINT('Origin',(0.,0.75,0.));
#16495=CARTESIAN_POINT('',(-0.8,0.75,9.79717439317883E-17));
#16496=CARTESIAN_POINT('Origin',(0.,0.75,0.));
#16497=CARTESIAN_POINT('',(0.562830534889751,0.75,0.238351419397483));
#16498=CARTESIAN_POINT('',(0.595438916863769,0.75,0.137993139022126));
#16499=CARTESIAN_POINT('Origin',(0.562758945330873,0.75,0.182851465569258));
#16500=CARTESIAN_POINT('',(0.608938287003997,0.75,0.0527614703521002));
#16501=CARTESIAN_POINT('Origin',(0.,0.75,0.));
#16502=CARTESIAN_POINT('',(0.608938287003997,0.75,-0.0527614703521002));
#16503=CARTESIAN_POINT('Origin',(0.591719772367581,0.75,0.));
#16504=CARTESIAN_POINT('',(0.595438916863769,0.75,-0.137993139022126));
#16505=CARTESIAN_POINT('Origin',(0.,0.75,0.));
#16506=CARTESIAN_POINT('',(0.562830534889751,0.75,-0.238351419397483));
#16507=CARTESIAN_POINT('Origin',(0.562758945330873,0.75,-0.182851465569258));
#16508=CARTESIAN_POINT('',(0.523653836874034,0.75,-0.315240018494132));
#16509=CARTESIAN_POINT('Origin',(0.,0.75,0.));
#16510=CARTESIAN_POINT('',(0.461629008549572,0.75,-0.40060987082025));
#16511=CARTESIAN_POINT('Origin',(0.478711351753049,0.75,-0.347804155687524));
#16512=CARTESIAN_POINT('',(0.40060987082025,0.75,-0.461629008549572));
#16513=CARTESIAN_POINT('Origin',(0.,0.75,0.));
#16514=CARTESIAN_POINT('',(0.315240018494132,0.75,-0.523653836874034));
#16515=CARTESIAN_POINT('Origin',(0.347804155687524,0.75,-0.478711351753049));
#16516=CARTESIAN_POINT('',(0.238351419397483,0.75,-0.562830534889751));
#16517=CARTESIAN_POINT('Origin',(0.,0.75,0.));
#16518=CARTESIAN_POINT('',(0.137993139022126,0.75,-0.595438916863769));
#16519=CARTESIAN_POINT('Origin',(0.182851465569258,0.75,-0.562758945330873));
#16520=CARTESIAN_POINT('',(0.0527614703521003,0.75,-0.608938287003997));
#16521=CARTESIAN_POINT('Origin',(0.,0.75,0.));
#16522=CARTESIAN_POINT('',(-0.0527614703521002,0.75,-0.608938287003997));
#16523=CARTESIAN_POINT('Origin',(3.6232386261108E-17,0.75,-0.591719772367581));
#16524=CARTESIAN_POINT('',(-0.137993139022126,0.75,-0.595438916863769));
#16525=CARTESIAN_POINT('Origin',(0.,0.75,0.));
#16526=CARTESIAN_POINT('',(-0.238351419397483,0.75,-0.562830534889751));
#16527=CARTESIAN_POINT('Origin',(-0.182851465569258,0.75,-0.562758945330873));
#16528=CARTESIAN_POINT('',(-0.315240018494132,0.75,-0.523653836874034));
#16529=CARTESIAN_POINT('Origin',(0.,0.75,0.));
#16530=CARTESIAN_POINT('',(-0.40060987082025,0.75,-0.461629008549572));
#16531=CARTESIAN_POINT('Origin',(-0.347804155687524,0.75,-0.478711351753049));
#16532=CARTESIAN_POINT('',(-0.461629008549572,0.75,-0.40060987082025));
#16533=CARTESIAN_POINT('Origin',(0.,0.75,0.));
#16534=CARTESIAN_POINT('',(-0.523653836874034,0.75,-0.315240018494132));
#16535=CARTESIAN_POINT('Origin',(-0.478711351753049,0.75,-0.347804155687524));
#16536=CARTESIAN_POINT('',(-0.562830534889751,0.75,-0.238351419397483));
#16537=CARTESIAN_POINT('Origin',(0.,0.75,0.));
#16538=CARTESIAN_POINT('',(-0.595438916863769,0.75,-0.137993139022126));
#16539=CARTESIAN_POINT('Origin',(-0.562758945330873,0.75,-0.182851465569258));
#16540=CARTESIAN_POINT('',(-0.608938287003997,0.75,-0.0527614703521003));
#16541=CARTESIAN_POINT('Origin',(0.,0.75,0.));
#16542=CARTESIAN_POINT('',(-0.608938287003997,0.75,0.0527614703521002));
#16543=CARTESIAN_POINT('Origin',(-0.591719772367581,0.75,-7.24647725222159E-17));
#16544=CARTESIAN_POINT('',(-0.595438916863769,0.75,0.137993139022126));
#16545=CARTESIAN_POINT('Origin',(0.,0.75,0.));
#16546=CARTESIAN_POINT('',(-0.562830534889751,0.75,0.238351419397483));
#16547=CARTESIAN_POINT('Origin',(-0.562758945330873,0.75,0.182851465569258));
#16548=CARTESIAN_POINT('',(-0.523653836874034,0.75,0.315240018494132));
#16549=CARTESIAN_POINT('Origin',(0.,0.75,0.));
#16550=CARTESIAN_POINT('',(-0.461629008549572,0.75,0.40060987082025));
#16551=CARTESIAN_POINT('Origin',(-0.478711351753049,0.75,0.347804155687524));
#16552=CARTESIAN_POINT('',(-0.40060987082025,0.75,0.461629008549572));
#16553=CARTESIAN_POINT('Origin',(0.,0.75,0.));
#16554=CARTESIAN_POINT('',(-0.315240018494132,0.75,0.523653836874034));
#16555=CARTESIAN_POINT('Origin',(-0.347804155687524,0.75,0.478711351753049));
#16556=CARTESIAN_POINT('',(-0.238351419397483,0.75,0.562830534889751));
#16557=CARTESIAN_POINT('Origin',(0.,0.75,0.));
#16558=CARTESIAN_POINT('',(-0.137993139022126,0.75,0.595438916863769));
#16559=CARTESIAN_POINT('Origin',(-0.182851465569258,0.75,0.562758945330873));
#16560=CARTESIAN_POINT('',(-0.0527614703521003,0.75,0.608938287003997));
#16561=CARTESIAN_POINT('Origin',(0.,0.75,0.));
#16562=CARTESIAN_POINT('',(0.0527614703521001,0.75,0.608938287003997));
#16563=CARTESIAN_POINT('Origin',(-1.08697158783324E-16,0.75,0.591719772367581));
#16564=CARTESIAN_POINT('',(0.137993139022126,0.75,0.595438916863769));
#16565=CARTESIAN_POINT('Origin',(0.,0.75,0.));
#16566=CARTESIAN_POINT('',(0.238351419397483,0.75,0.562830534889751));
#16567=CARTESIAN_POINT('Origin',(0.182851465569258,0.75,0.562758945330873));
#16568=CARTESIAN_POINT('',(0.315240018494132,0.75,0.523653836874034));
#16569=CARTESIAN_POINT('Origin',(0.,0.75,0.));
#16570=CARTESIAN_POINT('',(0.40060987082025,0.75,0.461629008549572));
#16571=CARTESIAN_POINT('Origin',(0.347804155687523,0.75,0.478711351753049));
#16572=CARTESIAN_POINT('',(0.461629008549572,0.75,0.40060987082025));
#16573=CARTESIAN_POINT('Origin',(0.,0.75,0.));
#16574=CARTESIAN_POINT('',(0.523653836874034,0.75,0.315240018494132));
#16575=CARTESIAN_POINT('Origin',(0.478711351753049,0.75,0.347804155687524));
#16576=CARTESIAN_POINT('Origin',(0.,0.75,0.));
#16577=CARTESIAN_POINT('Origin',(0.,0.75,0.));
#16578=CARTESIAN_POINT('',(-0.8,0.85,9.79717439317883E-17));
#16579=CARTESIAN_POINT('Origin',(0.,0.85,0.));
#16580=CARTESIAN_POINT('',(-0.8,0.75,9.79717439317883E-17));
#16581=CARTESIAN_POINT('Origin',(0.,0.85,0.));
#16582=CARTESIAN_POINT('Origin',(0.562758945330873,0.,0.182851465569258));
#16583=CARTESIAN_POINT('',(0.595438916863769,0.,0.137993139022126));
#16584=CARTESIAN_POINT('',(0.562830534889751,0.,0.238351419397483));
#16585=CARTESIAN_POINT('Origin',(0.,0.,0.));
#16586=CARTESIAN_POINT('',(0.523653836874034,0.,0.315240018494132));
#16587=CARTESIAN_POINT('Origin',(0.478711351753049,0.,0.347804155687524));
#16588=CARTESIAN_POINT('',(0.461629008549572,0.,0.40060987082025));
#16589=CARTESIAN_POINT('Origin',(0.,0.,0.));
#16590=CARTESIAN_POINT('',(0.40060987082025,0.,0.461629008549572));
#16591=CARTESIAN_POINT('Origin',(0.347804155687523,0.,0.478711351753049));
#16592=CARTESIAN_POINT('',(0.315240018494132,0.,0.523653836874034));
#16593=CARTESIAN_POINT('Origin',(0.,0.,0.));
#16594=CARTESIAN_POINT('',(0.238351419397483,0.,0.562830534889751));
#16595=CARTESIAN_POINT('Origin',(0.182851465569258,0.,0.562758945330873));
#16596=CARTESIAN_POINT('',(0.137993139022126,0.,0.595438916863769));
#16597=CARTESIAN_POINT('Origin',(0.,0.,0.));
#16598=CARTESIAN_POINT('',(0.0527614703521,0.,0.608938287003997));
#16599=CARTESIAN_POINT('Origin',(-1.08697158783324E-16,0.,0.591719772367581));
#16600=CARTESIAN_POINT('',(-0.0527614703521002,0.,0.608938287003997));
#16601=CARTESIAN_POINT('Origin',(0.,0.,0.));
#16602=CARTESIAN_POINT('',(-0.137993139022126,0.,0.595438916863769));
#16603=CARTESIAN_POINT('Origin',(-0.182851465569258,0.,0.562758945330873));
#16604=CARTESIAN_POINT('',(-0.238351419397483,0.,0.562830534889751));
#16605=CARTESIAN_POINT('Origin',(0.,0.,0.));
#16606=CARTESIAN_POINT('',(-0.315240018494132,0.,0.523653836874034));
#16607=CARTESIAN_POINT('Origin',(-0.347804155687524,0.,0.478711351753049));
#16608=CARTESIAN_POINT('',(-0.40060987082025,0.,0.461629008549572));
#16609=CARTESIAN_POINT('Origin',(0.,0.,0.));
#16610=CARTESIAN_POINT('',(-0.461629008549572,0.,0.40060987082025));
#16611=CARTESIAN_POINT('Origin',(-0.478711351753049,0.,0.347804155687524));
#16612=CARTESIAN_POINT('',(-0.523653836874034,0.,0.315240018494132));
#16613=CARTESIAN_POINT('Origin',(0.,0.,0.));
#16614=CARTESIAN_POINT('',(-0.562830534889751,0.,0.238351419397483));
#16615=CARTESIAN_POINT('Origin',(-0.562758945330873,0.,0.182851465569258));
#16616=CARTESIAN_POINT('',(-0.595438916863769,0.,0.137993139022126));
#16617=CARTESIAN_POINT('Origin',(0.,0.,0.));
#16618=CARTESIAN_POINT('',(-0.608938287003997,0.,0.0527614703521));
#16619=CARTESIAN_POINT('Origin',(-0.591719772367581,0.,-7.24647725222159E-17));
#16620=CARTESIAN_POINT('',(-0.608938287003997,0.,-0.0527614703521002));
#16621=CARTESIAN_POINT('Origin',(0.,0.,0.));
#16622=CARTESIAN_POINT('',(-0.595438916863769,0.,-0.137993139022126));
#16623=CARTESIAN_POINT('Origin',(-0.562758945330873,0.,-0.182851465569258));
#16624=CARTESIAN_POINT('',(-0.562830534889751,0.,-0.238351419397483));
#16625=CARTESIAN_POINT('Origin',(0.,0.,0.));
#16626=CARTESIAN_POINT('',(-0.523653836874034,0.,-0.315240018494132));
#16627=CARTESIAN_POINT('Origin',(-0.478711351753049,0.,-0.347804155687524));
#16628=CARTESIAN_POINT('',(-0.461629008549572,0.,-0.40060987082025));
#16629=CARTESIAN_POINT('Origin',(0.,0.,0.));
#16630=CARTESIAN_POINT('',(-0.40060987082025,0.,-0.461629008549572));
#16631=CARTESIAN_POINT('Origin',(-0.347804155687524,0.,-0.478711351753049));
#16632=CARTESIAN_POINT('',(-0.315240018494132,0.,-0.523653836874034));
#16633=CARTESIAN_POINT('Origin',(0.,0.,0.));
#16634=CARTESIAN_POINT('',(-0.238351419397483,0.,-0.562830534889751));
#16635=CARTESIAN_POINT('Origin',(-0.182851465569258,0.,-0.562758945330873));
#16636=CARTESIAN_POINT('',(-0.137993139022126,0.,-0.595438916863769));
#16637=CARTESIAN_POINT('Origin',(0.,0.,0.));
#16638=CARTESIAN_POINT('',(-0.0527614703521,0.,-0.608938287003997));
#16639=CARTESIAN_POINT('Origin',(3.6232386261108E-17,0.,-0.591719772367581));
#16640=CARTESIAN_POINT('',(0.0527614703521001,0.,-0.608938287003997));
#16641=CARTESIAN_POINT('Origin',(0.,0.,0.));
#16642=CARTESIAN_POINT('',(0.137993139022126,0.,-0.595438916863769));
#16643=CARTESIAN_POINT('Origin',(0.182851465569258,0.,-0.562758945330873));
#16644=CARTESIAN_POINT('',(0.238351419397483,0.,-0.562830534889751));
#16645=CARTESIAN_POINT('Origin',(0.,0.,0.));
#16646=CARTESIAN_POINT('',(0.315240018494132,0.,-0.523653836874034));
#16647=CARTESIAN_POINT('Origin',(0.347804155687524,0.,-0.478711351753049));
#16648=CARTESIAN_POINT('',(0.40060987082025,0.,-0.461629008549572));
#16649=CARTESIAN_POINT('Origin',(0.,0.,0.));
#16650=CARTESIAN_POINT('',(0.461629008549572,0.,-0.40060987082025));
#16651=CARTESIAN_POINT('Origin',(0.478711351753049,0.,-0.347804155687524));
#16652=CARTESIAN_POINT('',(0.523653836874034,0.,-0.315240018494132));
#16653=CARTESIAN_POINT('Origin',(0.,0.,0.));
#16654=CARTESIAN_POINT('',(0.562830534889751,0.,-0.238351419397483));
#16655=CARTESIAN_POINT('Origin',(0.562758945330873,0.,-0.182851465569258));
#16656=CARTESIAN_POINT('',(0.595438916863769,0.,-0.137993139022126));
#16657=CARTESIAN_POINT('Origin',(0.,0.,0.));
#16658=CARTESIAN_POINT('',(0.608938287003997,0.,0.0527614703521001));
#16659=CARTESIAN_POINT('Origin',(0.591719772367581,0.,0.));
#16660=CARTESIAN_POINT('',(0.608938287003997,0.,-0.0527614703521001));
#16661=CARTESIAN_POINT('Origin',(0.,0.,0.));
#16662=CARTESIAN_POINT('',(0.,0.,0.));
#16663=CARTESIAN_POINT('',(0.,0.,0.));
#16664=CARTESIAN_POINT('Origin',(6.97091003018116,-5.1,7.));
#16665=CARTESIAN_POINT('',(6.80591003018116,-5.,7.));
#16666=CARTESIAN_POINT('Origin',(6.97091003018116,-5.,7.));
#16667=CARTESIAN_POINT('',(6.80591003018116,-3.4,7.));
#16668=CARTESIAN_POINT('',(6.80591003018116,-5.1,7.));
#16669=CARTESIAN_POINT('Origin',(6.97091003018116,-3.4,7.));
#16670=CARTESIAN_POINT('Origin',(6.97091003018116,-3.4,7.));
#16671=CARTESIAN_POINT('Origin',(6.97091003018116,2.1,7.));
#16672=CARTESIAN_POINT('',(6.17091003018116,2.1,7.));
#16673=CARTESIAN_POINT('Origin',(6.97091003018116,2.1,7.));
#16674=CARTESIAN_POINT('',(6.37091003018116,2.1,7.));
#16675=CARTESIAN_POINT('Origin',(6.97091003018116,2.1,7.));
#16676=CARTESIAN_POINT('Origin',(6.97091003018116,1.4,7.));
#16677=CARTESIAN_POINT('',(6.17091003018116,1.4,7.));
#16678=CARTESIAN_POINT('Origin',(6.97091003018116,1.4,7.));
#16679=CARTESIAN_POINT('',(6.37091003018116,1.4,7.));
#16680=CARTESIAN_POINT('Origin',(6.97091003018116,1.4,7.));
#16681=CARTESIAN_POINT('Origin',(6.97091003018116,1.4,7.));
#16682=CARTESIAN_POINT('',(6.17091003018116,1.4,7.));
#16683=CARTESIAN_POINT('Origin',(6.97091003018116,-1.8,7.));
#16684=CARTESIAN_POINT('',(6.37091003018116,-5.,7.));
#16685=CARTESIAN_POINT('',(6.37091003018116,-1.8,7.));
#16686=CARTESIAN_POINT('Origin',(6.97091003018116,-5.,7.));
#16687=CARTESIAN_POINT('Origin',(6.97091003018116,-5.,7.));
#16688=CARTESIAN_POINT('Origin',(6.97091003018116,-1.8,7.));
#16689=CARTESIAN_POINT('',(6.37091003018116,3.,7.));
#16690=CARTESIAN_POINT('Origin',(6.97091003018116,3.,7.));
#16691=CARTESIAN_POINT('',(6.37091003018116,-1.8,7.));
#16692=CARTESIAN_POINT('Origin',(6.97091003018116,3.,7.));
#16693=CARTESIAN_POINT('',(0.,0.,0.));
#16694=CARTESIAN_POINT('Origin',(6.97091003018116,-2.65,7.));
#16695=CARTESIAN_POINT('',(6.36591003018116,-1.4,7.));
#16696=CARTESIAN_POINT('Origin',(6.97091003018116,-1.4,7.));
#16697=CARTESIAN_POINT('',(6.36591003018116,-2.65,7.));
#16698=CARTESIAN_POINT('',(6.36591003018116,-2.65,7.));
#16699=CARTESIAN_POINT('Origin',(6.97091003018116,-2.65,7.));
#16700=CARTESIAN_POINT('Origin',(6.97091003018116,-2.65,7.));
#16701=CARTESIAN_POINT('',(6.17091003018116,-1.4,7.));
#16702=CARTESIAN_POINT('Origin',(6.97091003018116,-1.4,7.));
#16703=CARTESIAN_POINT('',(6.17091003018116,-2.65,7.));
#16704=CARTESIAN_POINT('',(6.17091003018116,-2.65,7.));
#16705=CARTESIAN_POINT('Origin',(6.97091003018116,-2.65,7.));
#16706=CARTESIAN_POINT('Origin',(6.97091003018116,-1.4,7.));
#16707=CARTESIAN_POINT('Origin',(6.97091003018116,-2.65,7.));
#16708=CARTESIAN_POINT('',(0.,0.,0.));
#16709=CARTESIAN_POINT('Origin',(6.97091003018116,-0.4,7.));
#16710=CARTESIAN_POINT('',(6.36591003018116,0.4,7.));
#16711=CARTESIAN_POINT('Origin',(6.97091003018116,0.4,7.));
#16712=CARTESIAN_POINT('',(6.36591003018116,-0.4,7.));
#16713=CARTESIAN_POINT('',(6.36591003018116,-0.4,7.));
#16714=CARTESIAN_POINT('Origin',(6.97091003018116,-0.4,7.));
#16715=CARTESIAN_POINT('Origin',(6.97091003018116,-0.4,7.));
#16716=CARTESIAN_POINT('',(6.17091003018116,0.4,7.));
#16717=CARTESIAN_POINT('Origin',(6.97091003018116,0.4,7.));
#16718=CARTESIAN_POINT('',(6.17091003018116,-0.4,7.));
#16719=CARTESIAN_POINT('',(6.17091003018116,-0.4,7.));
#16720=CARTESIAN_POINT('Origin',(6.97091003018116,-0.4,7.));
#16721=CARTESIAN_POINT('Origin',(6.97091003018116,0.4,7.));
#16722=CARTESIAN_POINT('Origin',(6.97091003018116,-0.4,7.));
#16723=CARTESIAN_POINT('',(0.,0.,0.));
#16724=CARTESIAN_POINT('Origin',(6.97091003018116,-4.,6.));
#16725=CARTESIAN_POINT('',(6.82091003018116,-4.,6.4));
#16726=CARTESIAN_POINT('Origin',(6.97091003018116,-4.,6.4));
#16727=CARTESIAN_POINT('',(6.82091003018116,-4.,6.));
#16728=CARTESIAN_POINT('',(6.82091003018116,-4.,6.));
#16729=CARTESIAN_POINT('Origin',(6.97091003018116,-4.,6.));
#16730=CARTESIAN_POINT('Origin',(6.97091003018116,-4.,6.4));
#16731=CARTESIAN_POINT('Origin',(6.97091003018116,-4.,6.));
#16732=CARTESIAN_POINT('',(0.,0.,0.));
#16733=CARTESIAN_POINT('Origin',(6.97091003018116,-4.,7.6));
#16734=CARTESIAN_POINT('',(6.82091003018116,-4.,8.));
#16735=CARTESIAN_POINT('Origin',(6.97091003018116,-4.,8.));
#16736=CARTESIAN_POINT('',(6.82091003018116,-4.,7.6));
#16737=CARTESIAN_POINT('',(6.82091003018116,-4.,7.6));
#16738=CARTESIAN_POINT('Origin',(6.97091003018116,-4.,7.6));
#16739=CARTESIAN_POINT('Origin',(6.97091003018116,-4.,8.));
#16740=CARTESIAN_POINT('Origin',(6.97091003018116,-4.,7.6));
#16741=CARTESIAN_POINT('',(0.,0.,0.));
#16742=CARTESIAN_POINT('Origin',(6.97091003018116,-5.2,7.));
#16743=CARTESIAN_POINT('',(6.74591003018116,-5.,7.));
#16744=CARTESIAN_POINT('Origin',(6.97091003018116,-5.,7.));
#16745=CARTESIAN_POINT('',(6.74591003018116,-5.2,7.));
#16746=CARTESIAN_POINT('',(6.74591003018116,-5.2,7.));
#16747=CARTESIAN_POINT('Origin',(6.97091003018116,-5.2,7.));
#16748=CARTESIAN_POINT('Origin',(6.97091003018116,-5.2,7.));
#16749=CARTESIAN_POINT('',(6.17091003018116,-5.,7.));
#16750=CARTESIAN_POINT('Origin',(6.97091003018116,-5.,7.));
#16751=CARTESIAN_POINT('',(6.17091003018116,-5.2,7.));
#16752=CARTESIAN_POINT('',(6.17091003018116,-5.2,7.));
#16753=CARTESIAN_POINT('Origin',(6.97091003018116,-5.2,7.));
#16754=CARTESIAN_POINT('Origin',(6.97091003018116,-5.,7.));
#16755=CARTESIAN_POINT('Origin',(6.97091003018116,-5.2,7.));
#16756=CARTESIAN_POINT('',(0.,0.,0.));
#16757=CARTESIAN_POINT('Origin',(0.,-0.5,0.));
#16758=CARTESIAN_POINT('',(-1.,-0.375,-6.12323399573677E-17));
#16759=CARTESIAN_POINT('',(-0.992156741649222,-0.5,0.125));
#16760=CARTESIAN_POINT('Ctrl Pts',(-1.,-0.375,-1.00613961606655E-16));
#16761=CARTESIAN_POINT('Ctrl Pts',(-1.,-0.375,0.0157128711428661));
#16762=CARTESIAN_POINT('Ctrl Pts',(-0.999591823858855,-0.378143583103513,
0.0324619190698278));
#16763=CARTESIAN_POINT('Ctrl Pts',(-0.998116453123232,-0.390905426591754,
0.0632545375991437));
#16764=CARTESIAN_POINT('Ctrl Pts',(-0.997070068816062,-0.400522781657727,
0.0772994769543643));
#16765=CARTESIAN_POINT('Ctrl Pts',(-0.995102104277285,-0.422700615683787,
0.0994773109804239));
#16766=CARTESIAN_POINT('Ctrl Pts',(-0.994052129228928,-0.436745514765346,
0.109094593469654));
#16767=CARTESIAN_POINT('Ctrl Pts',(-0.99256853061881,-0.467537996927464,
0.121856383722779));
#16768=CARTESIAN_POINT('Ctrl Pts',(-0.992156741649222,-0.484286997589363,
0.125));
#16769=CARTESIAN_POINT('Ctrl Pts',(-0.992156741649222,-0.5,0.125));
#16770=CARTESIAN_POINT('',(-1.,-0.625,-6.12323399573677E-17));
#16771=CARTESIAN_POINT('Ctrl Pts',(-1.,-0.625,-4.5102810375397E-17));
#16772=CARTESIAN_POINT('Ctrl Pts',(-1.,-0.625,-0.0157128711428662));
#16773=CARTESIAN_POINT('Ctrl Pts',(-0.999591823858855,-0.621856416896487,
-0.032461919069828));
#16774=CARTESIAN_POINT('Ctrl Pts',(-0.998116453123232,-0.609094573408246,
-0.0632545375991439));
#16775=CARTESIAN_POINT('Ctrl Pts',(-0.997070068816062,-0.599477218342273,
-0.0772994769543645));
#16776=CARTESIAN_POINT('Ctrl Pts',(-0.995102104277285,-0.577299384316213,
-0.0994773109804241));
#16777=CARTESIAN_POINT('Ctrl Pts',(-0.994052129228928,-0.563254485234654,
-0.109094593469655));
#16778=CARTESIAN_POINT('Ctrl Pts',(-0.99256853061881,-0.532462003072536,
-0.121856383722779));
#16779=CARTESIAN_POINT('Ctrl Pts',(-0.992156741649221,-0.515713002410637,
-0.125));
#16780=CARTESIAN_POINT('Ctrl Pts',(-0.992156741649221,-0.484286997589363,
-0.125));
#16781=CARTESIAN_POINT('Ctrl Pts',(-0.99256853061881,-0.467537996927464,
-0.121856383722779));
#16782=CARTESIAN_POINT('Ctrl Pts',(-0.994052129228928,-0.436745514765346,
-0.109094593469655));
#16783=CARTESIAN_POINT('Ctrl Pts',(-0.995102104277285,-0.422700615683787,
-0.0994773109804241));
#16784=CARTESIAN_POINT('Ctrl Pts',(-0.997070068816062,-0.400522781657728,
-0.0772994769543645));
#16785=CARTESIAN_POINT('Ctrl Pts',(-0.998116453123232,-0.390905426591754,
-0.063254537599144));
#16786=CARTESIAN_POINT('Ctrl Pts',(-0.999591823858855,-0.378143583103513,
-0.0324619190698281));
#16787=CARTESIAN_POINT('Ctrl Pts',(-1.,-0.375,-0.0157128711428663));
#16788=CARTESIAN_POINT('Ctrl Pts',(-1.,-0.375,-9.36750677027476E-17));
#16789=CARTESIAN_POINT('Ctrl Pts',(-0.992156741649222,-0.5,0.125));
#16790=CARTESIAN_POINT('Ctrl Pts',(-0.992156741649222,-0.515713002410637,
0.125));
#16791=CARTESIAN_POINT('Ctrl Pts',(-0.99256853061881,-0.532462003072536,
0.121856383722779));
#16792=CARTESIAN_POINT('Ctrl Pts',(-0.994052129228928,-0.563254485234654,
0.109094593469654));
#16793=CARTESIAN_POINT('Ctrl Pts',(-0.995102104277285,-0.577299384316213,
0.0994773109804241));
#16794=CARTESIAN_POINT('Ctrl Pts',(-0.997070068816062,-0.599477218342273,
0.0772994769543644));
#16795=CARTESIAN_POINT('Ctrl Pts',(-0.998116453123232,-0.609094573408246,
0.0632545375991438));
#16796=CARTESIAN_POINT('Ctrl Pts',(-0.999591823858855,-0.621856416896487,
0.0324619190698279));
#16797=CARTESIAN_POINT('Ctrl Pts',(-1.,-0.625,0.0157128711428661));
#16798=CARTESIAN_POINT('Ctrl Pts',(-1.,-0.625,-4.85722573273506E-17));
#16799=CARTESIAN_POINT('',(-0.586834729715275,-0.5,0.125));
#16800=CARTESIAN_POINT('',(-7.65404249467096E-18,-0.5,0.125));
#16801=CARTESIAN_POINT('',(-0.6,-0.625,1.24532753107453E-17));
#16802=CARTESIAN_POINT('Ctrl Pts',(-0.6,-0.625,-4.16333634234434E-17));
#16803=CARTESIAN_POINT('Ctrl Pts',(-0.6,-0.625,0.0157444828659572));
#16804=CARTESIAN_POINT('Ctrl Pts',(-0.599317707212167,-0.621844041497889,
0.0325072544867633));
#16805=CARTESIAN_POINT('Ctrl Pts',(-0.596852269967858,-0.609072857638709,
0.0632914182239686));
#16806=CARTESIAN_POINT('Ctrl Pts',(-0.59510289473619,-0.599460146728784,
0.077316548567853));
#16807=CARTESIAN_POINT('Ctrl Pts',(-0.591804743154611,-0.577315815675743,
0.0994608796208941));
#16808=CARTESIAN_POINT('Ctrl Pts',(-0.590038488226116,-0.563290995658393,
0.109073016834181));
#16809=CARTESIAN_POINT('Ctrl Pts',(-0.587534197873268,-0.532507913768158,
0.121843784097853));
#16810=CARTESIAN_POINT('Ctrl Pts',(-0.586834729715275,-0.515745525063995,
0.125));
#16811=CARTESIAN_POINT('Ctrl Pts',(-0.586834729715275,-0.5,0.125));
#16812=CARTESIAN_POINT('',(-0.586834729715275,-0.5,-0.125));
#16813=CARTESIAN_POINT('Ctrl Pts',(-0.586834729715275,-0.5,-0.125));
#16814=CARTESIAN_POINT('Ctrl Pts',(-0.586834729715275,-0.515745525063995,
-0.125));
#16815=CARTESIAN_POINT('Ctrl Pts',(-0.587534197873268,-0.532507913768158,
-0.121843784097853));
#16816=CARTESIAN_POINT('Ctrl Pts',(-0.590038488226116,-0.563290995658393,
-0.109073016834181));
#16817=CARTESIAN_POINT('Ctrl Pts',(-0.591804743154611,-0.577315815675743,
-0.0994608796208942));
#16818=CARTESIAN_POINT('Ctrl Pts',(-0.59510289473619,-0.599460146728784,
-0.0773165485678531));
#16819=CARTESIAN_POINT('Ctrl Pts',(-0.596852269967858,-0.609072857638709,
-0.0632914182239687));
#16820=CARTESIAN_POINT('Ctrl Pts',(-0.599317707212167,-0.621844041497889,
-0.0325072544867635));
#16821=CARTESIAN_POINT('Ctrl Pts',(-0.6,-0.625,-0.0157444828659573));
#16822=CARTESIAN_POINT('Ctrl Pts',(-0.6,-0.625,-5.20417042793042E-17));
#16823=CARTESIAN_POINT('',(-0.6,-0.375,3.50046804984438E-17));
#16824=CARTESIAN_POINT('Ctrl Pts',(-0.6,-0.375,-3.46944695195361E-18));
#16825=CARTESIAN_POINT('Ctrl Pts',(-0.6,-0.375,-0.0157444828659572));
#16826=CARTESIAN_POINT('Ctrl Pts',(-0.599317707212167,-0.378155958502111,
-0.0325072544867634));
#16827=CARTESIAN_POINT('Ctrl Pts',(-0.596852269967858,-0.390927142361291,
-0.0632914182239686));
#16828=CARTESIAN_POINT('Ctrl Pts',(-0.59510289473619,-0.400539853271216,
-0.077316548567853));
#16829=CARTESIAN_POINT('Ctrl Pts',(-0.591804743154611,-0.422684184324257,
-0.0994608796208942));
#16830=CARTESIAN_POINT('Ctrl Pts',(-0.590038488226116,-0.436709004341607,
-0.109073016834181));
#16831=CARTESIAN_POINT('Ctrl Pts',(-0.587534197873268,-0.467492086231842,
-0.121843784097853));
#16832=CARTESIAN_POINT('Ctrl Pts',(-0.586834729715275,-0.484254474936005,
-0.125));
#16833=CARTESIAN_POINT('Ctrl Pts',(-0.586834729715275,-0.5,-0.125));
#16834=CARTESIAN_POINT('Ctrl Pts',(-0.586834729715275,-0.5,0.125));
#16835=CARTESIAN_POINT('Ctrl Pts',(-0.586834729715275,-0.484254474936005,
0.125));
#16836=CARTESIAN_POINT('Ctrl Pts',(-0.587534197873268,-0.467492086231842,
0.121843784097853));
#16837=CARTESIAN_POINT('Ctrl Pts',(-0.590038488226116,-0.436709004341607,
0.109073016834181));
#16838=CARTESIAN_POINT('Ctrl Pts',(-0.591804743154611,-0.422684184324257,
0.0994608796208941));
#16839=CARTESIAN_POINT('Ctrl Pts',(-0.59510289473619,-0.400539853271216,
0.077316548567853));
#16840=CARTESIAN_POINT('Ctrl Pts',(-0.596852269967858,-0.390927142361291,
0.0632914182239686));
#16841=CARTESIAN_POINT('Ctrl Pts',(-0.599317707212167,-0.378155958502111,
0.0325072544867634));
#16842=CARTESIAN_POINT('Ctrl Pts',(-0.6,-0.375,0.0157444828659572));
#16843=CARTESIAN_POINT('Ctrl Pts',(-0.6,-0.375,-2.42861286636753E-17));
#16844=CARTESIAN_POINT('Origin',(0.,-0.5,0.));
#16845=CARTESIAN_POINT('',(0.586834729715275,-0.5,-0.125));
#16846=CARTESIAN_POINT('',(0.586834729715275,-0.5,0.125));
#16847=CARTESIAN_POINT('Ctrl Pts',(0.586834729715275,-0.5,-0.125));
#16848=CARTESIAN_POINT('Ctrl Pts',(0.586834729715275,-0.484254474936005,
-0.125));
#16849=CARTESIAN_POINT('Ctrl Pts',(0.587534197873268,-0.467492086231842,
-0.121843784097853));
#16850=CARTESIAN_POINT('Ctrl Pts',(0.590038488226116,-0.436709004341607,
-0.109073016834181));
#16851=CARTESIAN_POINT('Ctrl Pts',(0.591804743154611,-0.422684184324257,
-0.0994608796208941));
#16852=CARTESIAN_POINT('Ctrl Pts',(0.59510289473619,-0.400539853271216,
-0.0773165485678529));
#16853=CARTESIAN_POINT('Ctrl Pts',(0.596852269967858,-0.390927142361291,
-0.0632914182239686));
#16854=CARTESIAN_POINT('Ctrl Pts',(0.599317707212167,-0.378155958502111,
-0.0325072544867633));
#16855=CARTESIAN_POINT('Ctrl Pts',(0.6,-0.375,-0.0157444828659572));
#16856=CARTESIAN_POINT('Ctrl Pts',(0.6,-0.375,0.0157444828659573));
#16857=CARTESIAN_POINT('Ctrl Pts',(0.599317707212167,-0.378155958502111,
0.0325072544867635));
#16858=CARTESIAN_POINT('Ctrl Pts',(0.596852269967858,-0.390927142361291,
0.0632914182239687));
#16859=CARTESIAN_POINT('Ctrl Pts',(0.59510289473619,-0.400539853271216,
0.0773165485678531));
#16860=CARTESIAN_POINT('Ctrl Pts',(0.591804743154611,-0.422684184324257,
0.0994608796208942));
#16861=CARTESIAN_POINT('Ctrl Pts',(0.590038488226116,-0.436709004341607,
0.109073016834181));
#16862=CARTESIAN_POINT('Ctrl Pts',(0.587534197873268,-0.467492086231842,
0.121843784097853));
#16863=CARTESIAN_POINT('Ctrl Pts',(0.586834729715275,-0.484254474936005,
0.125));
#16864=CARTESIAN_POINT('Ctrl Pts',(0.586834729715275,-0.5,0.125));
#16865=CARTESIAN_POINT('Ctrl Pts',(0.586834729715275,-0.5,0.125));
#16866=CARTESIAN_POINT('Ctrl Pts',(0.586834729715275,-0.515745525063995,
0.125));
#16867=CARTESIAN_POINT('Ctrl Pts',(0.587534197873268,-0.532507913768158,
0.121843784097853));
#16868=CARTESIAN_POINT('Ctrl Pts',(0.590038488226116,-0.563290995658393,
0.109073016834181));
#16869=CARTESIAN_POINT('Ctrl Pts',(0.591804743154611,-0.577315815675743,
0.0994608796208942));
#16870=CARTESIAN_POINT('Ctrl Pts',(0.59510289473619,-0.599460146728784,
0.077316548567853));
#16871=CARTESIAN_POINT('Ctrl Pts',(0.596852269967858,-0.609072857638709,
0.0632914182239688));
#16872=CARTESIAN_POINT('Ctrl Pts',(0.599317707212167,-0.621844041497889,
0.0325072544867635));
#16873=CARTESIAN_POINT('Ctrl Pts',(0.6,-0.625,0.0157444828659573));
#16874=CARTESIAN_POINT('Ctrl Pts',(0.6,-0.625,-0.0157444828659572));
#16875=CARTESIAN_POINT('Ctrl Pts',(0.599317707212167,-0.621844041497889,
-0.0325072544867633));
#16876=CARTESIAN_POINT('Ctrl Pts',(0.596852269967858,-0.609072857638709,
-0.0632914182239685));
#16877=CARTESIAN_POINT('Ctrl Pts',(0.59510289473619,-0.599460146728784,
-0.077316548567853));
#16878=CARTESIAN_POINT('Ctrl Pts',(0.591804743154611,-0.577315815675743,
-0.0994608796208941));
#16879=CARTESIAN_POINT('Ctrl Pts',(0.590038488226116,-0.563290995658393,
-0.10907301683418));
#16880=CARTESIAN_POINT('Ctrl Pts',(0.587534197873268,-0.532507913768158,
-0.121843784097853));
#16881=CARTESIAN_POINT('Ctrl Pts',(0.586834729715275,-0.515745525063995,
-0.125));
#16882=CARTESIAN_POINT('Ctrl Pts',(0.586834729715275,-0.5,-0.125));
#16883=CARTESIAN_POINT('',(0.992156741649222,-0.5,0.125));
#16884=CARTESIAN_POINT('',(-7.65404249467096E-18,-0.5,0.125));
#16885=CARTESIAN_POINT('',(1.,-0.625,6.12323399573677E-17));
#16886=CARTESIAN_POINT('Ctrl Pts',(1.,-0.625,7.28583859910259E-17));
#16887=CARTESIAN_POINT('Ctrl Pts',(1.,-0.625,0.0157128711428663));
#16888=CARTESIAN_POINT('Ctrl Pts',(0.999591823858855,-0.621856416896487,
0.032461919069828));
#16889=CARTESIAN_POINT('Ctrl Pts',(0.998116453123232,-0.609094573408246,
0.0632545375991439));
#16890=CARTESIAN_POINT('Ctrl Pts',(0.997070068816062,-0.599477218342273,
0.0772994769543645));
#16891=CARTESIAN_POINT('Ctrl Pts',(0.995102104277285,-0.577299384316213,
0.0994773109804242));
#16892=CARTESIAN_POINT('Ctrl Pts',(0.994052129228928,-0.563254485234654,
0.109094593469655));
#16893=CARTESIAN_POINT('Ctrl Pts',(0.99256853061881,-0.532462003072536,
0.121856383722779));
#16894=CARTESIAN_POINT('Ctrl Pts',(0.992156741649222,-0.515713002410637,
0.125));
#16895=CARTESIAN_POINT('Ctrl Pts',(0.992156741649222,-0.5,0.125));
#16896=CARTESIAN_POINT('',(1.,-0.375,6.12323399573677E-17));
#16897=CARTESIAN_POINT('Ctrl Pts',(1.,-0.375,2.08166817117217E-17));
#16898=CARTESIAN_POINT('Ctrl Pts',(1.,-0.375,-0.0157128711428662));
#16899=CARTESIAN_POINT('Ctrl Pts',(0.999591823858855,-0.378143583103513,
-0.032461919069828));
#16900=CARTESIAN_POINT('Ctrl Pts',(0.998116453123232,-0.390905426591754,
-0.0632545375991438));
#16901=CARTESIAN_POINT('Ctrl Pts',(0.997070068816062,-0.400522781657728,
-0.0772994769543644));
#16902=CARTESIAN_POINT('Ctrl Pts',(0.995102104277285,-0.422700615683787,
-0.099477310980424));
#16903=CARTESIAN_POINT('Ctrl Pts',(0.994052129228928,-0.436745514765346,
-0.109094593469654));
#16904=CARTESIAN_POINT('Ctrl Pts',(0.99256853061881,-0.467537996927464,
-0.121856383722779));
#16905=CARTESIAN_POINT('Ctrl Pts',(0.992156741649222,-0.484286997589363,
-0.125));
#16906=CARTESIAN_POINT('Ctrl Pts',(0.992156741649222,-0.515713002410637,
-0.125));
#16907=CARTESIAN_POINT('Ctrl Pts',(0.99256853061881,-0.532462003072536,
-0.121856383722779));
#16908=CARTESIAN_POINT('Ctrl Pts',(0.994052129228928,-0.563254485234654,
-0.109094593469654));
#16909=CARTESIAN_POINT('Ctrl Pts',(0.995102104277285,-0.577299384316213,
-0.099477310980424));
#16910=CARTESIAN_POINT('Ctrl Pts',(0.997070068816062,-0.599477218342273,
-0.0772994769543643));
#16911=CARTESIAN_POINT('Ctrl Pts',(0.998116453123232,-0.609094573408246,
-0.0632545375991438));
#16912=CARTESIAN_POINT('Ctrl Pts',(0.999591823858855,-0.621856416896487,
-0.0324619190698279));
#16913=CARTESIAN_POINT('Ctrl Pts',(1.,-0.625,-0.0157128711428661));
#16914=CARTESIAN_POINT('Ctrl Pts',(1.,-0.625,8.32667268468867E-17));
#16915=CARTESIAN_POINT('Ctrl Pts',(0.992156741649222,-0.5,0.125));
#16916=CARTESIAN_POINT('Ctrl Pts',(0.992156741649222,-0.484286997589363,
0.125));
#16917=CARTESIAN_POINT('Ctrl Pts',(0.99256853061881,-0.467537996927464,
0.121856383722779));
#16918=CARTESIAN_POINT('Ctrl Pts',(0.994052129228928,-0.436745514765346,
0.109094593469654));
#16919=CARTESIAN_POINT('Ctrl Pts',(0.995102104277285,-0.422700615683787,
0.0994773109804241));
#16920=CARTESIAN_POINT('Ctrl Pts',(0.997070068816062,-0.400522781657727,
0.0772994769543644));
#16921=CARTESIAN_POINT('Ctrl Pts',(0.998116453123232,-0.390905426591754,
0.0632545375991438));
#16922=CARTESIAN_POINT('Ctrl Pts',(0.999591823858855,-0.378143583103513,
0.0324619190698279));
#16923=CARTESIAN_POINT('Ctrl Pts',(1.,-0.375,0.0157128711428662));
#16924=CARTESIAN_POINT('Ctrl Pts',(1.,-0.375,2.77555756156289E-17));
#16925=CARTESIAN_POINT('Origin',(0.,-0.1,0.));
#16926=CARTESIAN_POINT('',(-1.,-0.9,1.22464679914735E-16));
#16927=CARTESIAN_POINT('Origin',(0.,-0.9,0.));
#16928=CARTESIAN_POINT('',(-1.,-0.1,-1.22464679914735E-16));
#16929=CARTESIAN_POINT('',(-1.,-0.1,1.22464679914735E-16));
#16930=CARTESIAN_POINT('',(-1.,-0.1,-1.22464679914735E-16));
#16931=CARTESIAN_POINT('Origin',(0.,-0.1,0.));
#16932=CARTESIAN_POINT('',(0.,-0.625,-1.));
#16933=CARTESIAN_POINT('',(0.,-0.375,-1.));
#16934=CARTESIAN_POINT('Ctrl Pts',(-2.08166817117217E-17,-0.625,-1.));
#16935=CARTESIAN_POINT('Ctrl Pts',(0.0157128711428662,-0.625,-1.));
#16936=CARTESIAN_POINT('Ctrl Pts',(0.0324619190698279,-0.621856416896487,
-0.999591823858855));
#16937=CARTESIAN_POINT('Ctrl Pts',(0.0632545375991438,-0.609094573408246,
-0.998116453123232));
#16938=CARTESIAN_POINT('Ctrl Pts',(0.0772994769543644,-0.599477218342273,
-0.997070068816062));
#16939=CARTESIAN_POINT('Ctrl Pts',(0.0994773109804241,-0.577299384316213,
-0.995102104277285));
#16940=CARTESIAN_POINT('Ctrl Pts',(0.109094593469654,-0.563254485234654,
-0.994052129228928));
#16941=CARTESIAN_POINT('Ctrl Pts',(0.121856383722779,-0.532462003072536,
-0.99256853061881));
#16942=CARTESIAN_POINT('Ctrl Pts',(0.125,-0.515713002410637,-0.992156741649221));
#16943=CARTESIAN_POINT('Ctrl Pts',(0.125,-0.484286997589363,-0.992156741649221));
#16944=CARTESIAN_POINT('Ctrl Pts',(0.121856383722779,-0.467537996927464,
-0.99256853061881));
#16945=CARTESIAN_POINT('Ctrl Pts',(0.109094593469654,-0.436745514765346,
-0.994052129228928));
#16946=CARTESIAN_POINT('Ctrl Pts',(0.0994773109804241,-0.422700615683787,
-0.995102104277285));
#16947=CARTESIAN_POINT('Ctrl Pts',(0.0772994769543645,-0.400522781657728,
-0.997070068816062));
#16948=CARTESIAN_POINT('Ctrl Pts',(0.0632545375991439,-0.390905426591754,
-0.998116453123232));
#16949=CARTESIAN_POINT('Ctrl Pts',(0.032461919069828,-0.378143583103513,
-0.999591823858855));
#16950=CARTESIAN_POINT('Ctrl Pts',(0.0157128711428662,-0.375,-1.));
#16951=CARTESIAN_POINT('Ctrl Pts',(3.81639164714898E-17,-0.375,-1.));
#16952=CARTESIAN_POINT('',(-0.125,-0.5,-0.992156741649222));
#16953=CARTESIAN_POINT('Ctrl Pts',(4.5102810375397E-17,-0.375,-1.));
#16954=CARTESIAN_POINT('Ctrl Pts',(-0.0157128711428661,-0.375,-1.));
#16955=CARTESIAN_POINT('Ctrl Pts',(-0.0324619190698279,-0.378143583103513,
-0.999591823858855));
#16956=CARTESIAN_POINT('Ctrl Pts',(-0.0632545375991437,-0.390905426591754,
-0.998116453123232));
#16957=CARTESIAN_POINT('Ctrl Pts',(-0.0772994769543643,-0.400522781657727,
-0.997070068816062));
#16958=CARTESIAN_POINT('Ctrl Pts',(-0.099477310980424,-0.422700615683787,
-0.995102104277285));
#16959=CARTESIAN_POINT('Ctrl Pts',(-0.109094593469654,-0.436745514765346,
-0.994052129228928));
#16960=CARTESIAN_POINT('Ctrl Pts',(-0.121856383722779,-0.467537996927464,
-0.99256853061881));
#16961=CARTESIAN_POINT('Ctrl Pts',(-0.125,-0.484286997589363,-0.992156741649222));
#16962=CARTESIAN_POINT('Ctrl Pts',(-0.125,-0.5,-0.992156741649222));
#16963=CARTESIAN_POINT('Ctrl Pts',(-0.125,-0.5,-0.992156741649222));
#16964=CARTESIAN_POINT('Ctrl Pts',(-0.125,-0.515713002410637,-0.992156741649222));
#16965=CARTESIAN_POINT('Ctrl Pts',(-0.121856383722779,-0.532462003072536,
-0.99256853061881));
#16966=CARTESIAN_POINT('Ctrl Pts',(-0.109094593469654,-0.563254485234654,
-0.994052129228928));
#16967=CARTESIAN_POINT('Ctrl Pts',(-0.0994773109804241,-0.577299384316213,
-0.995102104277285));
#16968=CARTESIAN_POINT('Ctrl Pts',(-0.0772994769543644,-0.599477218342273,
-0.997070068816062));
#16969=CARTESIAN_POINT('Ctrl Pts',(-0.0632545375991439,-0.609094573408246,
-0.998116453123232));
#16970=CARTESIAN_POINT('Ctrl Pts',(-0.032461919069828,-0.621856416896487,
-0.999591823858855));
#16971=CARTESIAN_POINT('Ctrl Pts',(-0.0157128711428662,-0.625,-1.));
#16972=CARTESIAN_POINT('Ctrl Pts',(-1.38777878078145E-17,-0.625,-1.));
#16973=CARTESIAN_POINT('',(0.,-0.375,1.));
#16974=CARTESIAN_POINT('',(0.,-0.625,1.));
#16975=CARTESIAN_POINT('Ctrl Pts',(4.16333634234434E-17,-0.375,1.));
#16976=CARTESIAN_POINT('Ctrl Pts',(0.0157128711428662,-0.375,1.));
#16977=CARTESIAN_POINT('Ctrl Pts',(0.032461919069828,-0.378143583103513,
0.999591823858855));
#16978=CARTESIAN_POINT('Ctrl Pts',(0.0632545375991439,-0.390905426591754,
0.998116453123232));
#16979=CARTESIAN_POINT('Ctrl Pts',(0.0772994769543644,-0.400522781657728,
0.997070068816062));
#16980=CARTESIAN_POINT('Ctrl Pts',(0.0994773109804241,-0.422700615683787,
0.995102104277285));
#16981=CARTESIAN_POINT('Ctrl Pts',(0.109094593469654,-0.436745514765346,
0.994052129228928));
#16982=CARTESIAN_POINT('Ctrl Pts',(0.121856383722779,-0.467537996927464,
0.99256853061881));
#16983=CARTESIAN_POINT('Ctrl Pts',(0.125,-0.484286997589363,0.992156741649222));
#16984=CARTESIAN_POINT('Ctrl Pts',(0.125,-0.515713002410637,0.992156741649222));
#16985=CARTESIAN_POINT('Ctrl Pts',(0.121856383722779,-0.532462003072536,
0.99256853061881));
#16986=CARTESIAN_POINT('Ctrl Pts',(0.109094593469655,-0.563254485234654,
0.994052129228928));
#16987=CARTESIAN_POINT('Ctrl Pts',(0.0994773109804241,-0.577299384316213,
0.995102104277285));
#16988=CARTESIAN_POINT('Ctrl Pts',(0.0772994769543644,-0.599477218342273,
0.997070068816062));
#16989=CARTESIAN_POINT('Ctrl Pts',(0.0632545375991438,-0.609094573408246,
0.998116453123232));
#16990=CARTESIAN_POINT('Ctrl Pts',(0.0324619190698279,-0.621856416896487,
0.999591823858855));
#16991=CARTESIAN_POINT('Ctrl Pts',(0.0157128711428662,-0.625,1.));
#16992=CARTESIAN_POINT('Ctrl Pts',(-1.73472347597681E-17,-0.625,1.));
#16993=CARTESIAN_POINT('',(-0.125,-0.5,0.992156741649222));
#16994=CARTESIAN_POINT('Ctrl Pts',(-1.73472347597681E-17,-0.625,1.));
#16995=CARTESIAN_POINT('Ctrl Pts',(-0.0157128711428662,-0.625,1.));
#16996=CARTESIAN_POINT('Ctrl Pts',(-0.032461919069828,-0.621856416896487,
0.999591823858855));
#16997=CARTESIAN_POINT('Ctrl Pts',(-0.0632545375991439,-0.609094573408246,
0.998116453123232));
#16998=CARTESIAN_POINT('Ctrl Pts',(-0.0772994769543645,-0.599477218342273,
0.997070068816062));
#16999=CARTESIAN_POINT('Ctrl Pts',(-0.0994773109804241,-0.577299384316213,
0.995102104277285));
#17000=CARTESIAN_POINT('Ctrl Pts',(-0.109094593469654,-0.563254485234654,
0.994052129228928));
#17001=CARTESIAN_POINT('Ctrl Pts',(-0.121856383722779,-0.532462003072536,
0.99256853061881));
#17002=CARTESIAN_POINT('Ctrl Pts',(-0.125,-0.515713002410637,0.992156741649222));
#17003=CARTESIAN_POINT('Ctrl Pts',(-0.125,-0.5,0.992156741649222));
#17004=CARTESIAN_POINT('Ctrl Pts',(-0.125,-0.5,0.992156741649222));
#17005=CARTESIAN_POINT('Ctrl Pts',(-0.125,-0.484286997589363,0.992156741649222));
#17006=CARTESIAN_POINT('Ctrl Pts',(-0.121856383722779,-0.467537996927464,
0.99256853061881));
#17007=CARTESIAN_POINT('Ctrl Pts',(-0.109094593469654,-0.436745514765346,
0.994052129228928));
#17008=CARTESIAN_POINT('Ctrl Pts',(-0.099477310980424,-0.422700615683787,
0.995102104277285));
#17009=CARTESIAN_POINT('Ctrl Pts',(-0.0772994769543643,-0.400522781657727,
0.997070068816062));
#17010=CARTESIAN_POINT('Ctrl Pts',(-0.0632545375991438,-0.390905426591754,
0.998116453123232));
#17011=CARTESIAN_POINT('Ctrl Pts',(-0.0324619190698279,-0.378143583103513,
0.999591823858855));
#17012=CARTESIAN_POINT('Ctrl Pts',(-0.0157128711428661,-0.375,1.));
#17013=CARTESIAN_POINT('Ctrl Pts',(4.5102810375397E-17,-0.375,1.));
#17014=CARTESIAN_POINT('Origin',(0.,-0.5,0.));
#17015=CARTESIAN_POINT('',(-0.125,-0.5,-0.586834729715275));
#17016=CARTESIAN_POINT('',(-0.125,-0.5,0.));
#17017=CARTESIAN_POINT('',(0.125,-0.5,-0.586834729715275));
#17018=CARTESIAN_POINT('Ctrl Pts',(0.125,-0.5,-0.586834729715275));
#17019=CARTESIAN_POINT('Ctrl Pts',(0.125,-0.515745525063995,-0.586834729715275));
#17020=CARTESIAN_POINT('Ctrl Pts',(0.121843784097853,-0.532507913768158,
-0.587534197873268));
#17021=CARTESIAN_POINT('Ctrl Pts',(0.109073016834181,-0.563290995658393,
-0.590038488226116));
#17022=CARTESIAN_POINT('Ctrl Pts',(0.0994608796208942,-0.577315815675743,
-0.591804743154611));
#17023=CARTESIAN_POINT('Ctrl Pts',(0.077316548567853,-0.599460146728784,
-0.59510289473619));
#17024=CARTESIAN_POINT('Ctrl Pts',(0.0632914182239686,-0.609072857638709,
-0.596852269967858));
#17025=CARTESIAN_POINT('Ctrl Pts',(0.0325072544867633,-0.621844041497889,
-0.599317707212167));
#17026=CARTESIAN_POINT('Ctrl Pts',(0.0157444828659573,-0.625,-0.6));
#17027=CARTESIAN_POINT('Ctrl Pts',(-0.0157444828659572,-0.625,-0.6));
#17028=CARTESIAN_POINT('Ctrl Pts',(-0.0325072544867633,-0.621844041497889,
-0.599317707212167));
#17029=CARTESIAN_POINT('Ctrl Pts',(-0.0632914182239686,-0.609072857638709,
-0.596852269967858));
#17030=CARTESIAN_POINT('Ctrl Pts',(-0.077316548567853,-0.599460146728784,
-0.59510289473619));
#17031=CARTESIAN_POINT('Ctrl Pts',(-0.0994608796208941,-0.577315815675743,
-0.591804743154611));
#17032=CARTESIAN_POINT('Ctrl Pts',(-0.109073016834181,-0.563290995658393,
-0.590038488226116));
#17033=CARTESIAN_POINT('Ctrl Pts',(-0.121843784097853,-0.532507913768158,
-0.587534197873268));
#17034=CARTESIAN_POINT('Ctrl Pts',(-0.125,-0.515745525063995,-0.586834729715275));
#17035=CARTESIAN_POINT('Ctrl Pts',(-0.125,-0.5,-0.586834729715275));
#17036=CARTESIAN_POINT('Ctrl Pts',(-0.125,-0.5,-0.586834729715275));
#17037=CARTESIAN_POINT('Ctrl Pts',(-0.125,-0.484254474936005,-0.586834729715275));
#17038=CARTESIAN_POINT('Ctrl Pts',(-0.121843784097853,-0.467492086231842,
-0.587534197873268));
#17039=CARTESIAN_POINT('Ctrl Pts',(-0.109073016834181,-0.436709004341607,
-0.590038488226116));
#17040=CARTESIAN_POINT('Ctrl Pts',(-0.0994608796208942,-0.422684184324257,
-0.591804743154611));
#17041=CARTESIAN_POINT('Ctrl Pts',(-0.077316548567853,-0.400539853271216,
-0.59510289473619));
#17042=CARTESIAN_POINT('Ctrl Pts',(-0.0632914182239687,-0.39092714236129,
-0.596852269967858));
#17043=CARTESIAN_POINT('Ctrl Pts',(-0.0325072544867634,-0.378155958502111,
-0.599317707212167));
#17044=CARTESIAN_POINT('Ctrl Pts',(-0.0157444828659573,-0.375,-0.6));
#17045=CARTESIAN_POINT('Ctrl Pts',(0.0157444828659572,-0.375,-0.6));
#17046=CARTESIAN_POINT('Ctrl Pts',(0.0325072544867634,-0.378155958502111,
-0.599317707212167));
#17047=CARTESIAN_POINT('Ctrl Pts',(0.0632914182239686,-0.390927142361291,
-0.596852269967858));
#17048=CARTESIAN_POINT('Ctrl Pts',(0.077316548567853,-0.400539853271216,
-0.59510289473619));
#17049=CARTESIAN_POINT('Ctrl Pts',(0.0994608796208941,-0.422684184324257,
-0.591804743154611));
#17050=CARTESIAN_POINT('Ctrl Pts',(0.109073016834181,-0.436709004341607,
-0.590038488226116));
#17051=CARTESIAN_POINT('Ctrl Pts',(0.121843784097853,-0.467492086231842,
-0.587534197873268));
#17052=CARTESIAN_POINT('Ctrl Pts',(0.125,-0.484254474936005,-0.586834729715275));
#17053=CARTESIAN_POINT('Ctrl Pts',(0.125,-0.5,-0.586834729715275));
#17054=CARTESIAN_POINT('Origin',(0.,-0.5,0.));
#17055=CARTESIAN_POINT('',(0.125,-0.5,0.586834729715275));
#17056=CARTESIAN_POINT('',(-0.125,-0.5,0.586834729715275));
#17057=CARTESIAN_POINT('Ctrl Pts',(0.125,-0.5,0.586834729715275));
#17058=CARTESIAN_POINT('Ctrl Pts',(0.125,-0.484254474936005,0.586834729715275));
#17059=CARTESIAN_POINT('Ctrl Pts',(0.121843784097853,-0.467492086231842,
0.587534197873268));
#17060=CARTESIAN_POINT('Ctrl Pts',(0.109073016834181,-0.436709004341607,
0.590038488226116));
#17061=CARTESIAN_POINT('Ctrl Pts',(0.0994608796208941,-0.422684184324257,
0.591804743154611));
#17062=CARTESIAN_POINT('Ctrl Pts',(0.077316548567853,-0.400539853271216,
0.59510289473619));
#17063=CARTESIAN_POINT('Ctrl Pts',(0.0632914182239686,-0.390927142361291,
0.596852269967858));
#17064=CARTESIAN_POINT('Ctrl Pts',(0.0325072544867634,-0.378155958502111,
0.599317707212167));
#17065=CARTESIAN_POINT('Ctrl Pts',(0.0157444828659572,-0.375,0.6));
#17066=CARTESIAN_POINT('Ctrl Pts',(-0.0157444828659573,-0.375,0.6));
#17067=CARTESIAN_POINT('Ctrl Pts',(-0.0325072544867634,-0.378155958502111,
0.599317707212167));
#17068=CARTESIAN_POINT('Ctrl Pts',(-0.0632914182239687,-0.390927142361291,
0.596852269967858));
#17069=CARTESIAN_POINT('Ctrl Pts',(-0.077316548567853,-0.400539853271216,
0.59510289473619));
#17070=CARTESIAN_POINT('Ctrl Pts',(-0.0994608796208942,-0.422684184324257,
0.591804743154611));
#17071=CARTESIAN_POINT('Ctrl Pts',(-0.109073016834181,-0.436709004341607,
0.590038488226116));
#17072=CARTESIAN_POINT('Ctrl Pts',(-0.121843784097853,-0.467492086231842,
0.587534197873268));
#17073=CARTESIAN_POINT('Ctrl Pts',(-0.125,-0.484254474936005,0.586834729715275));
#17074=CARTESIAN_POINT('Ctrl Pts',(-0.125,-0.5,0.586834729715275));
#17075=CARTESIAN_POINT('Ctrl Pts',(-0.125,-0.5,0.586834729715275));
#17076=CARTESIAN_POINT('Ctrl Pts',(-0.125,-0.515745525063995,0.586834729715275));
#17077=CARTESIAN_POINT('Ctrl Pts',(-0.121843784097853,-0.532507913768158,
0.587534197873268));
#17078=CARTESIAN_POINT('Ctrl Pts',(-0.109073016834181,-0.563290995658393,
0.590038488226116));
#17079=CARTESIAN_POINT('Ctrl Pts',(-0.0994608796208941,-0.577315815675743,
0.591804743154611));
#17080=CARTESIAN_POINT('Ctrl Pts',(-0.077316548567853,-0.599460146728784,
0.59510289473619));
#17081=CARTESIAN_POINT('Ctrl Pts',(-0.0632914182239687,-0.609072857638709,
0.596852269967858));
#17082=CARTESIAN_POINT('Ctrl Pts',(-0.0325072544867635,-0.621844041497889,
0.599317707212167));
#17083=CARTESIAN_POINT('Ctrl Pts',(-0.0157444828659572,-0.625,0.6));
#17084=CARTESIAN_POINT('Ctrl Pts',(0.0157444828659572,-0.625,0.6));
#17085=CARTESIAN_POINT('Ctrl Pts',(0.0325072544867633,-0.621844041497889,
0.599317707212167));
#17086=CARTESIAN_POINT('Ctrl Pts',(0.0632914182239686,-0.609072857638709,
0.596852269967858));
#17087=CARTESIAN_POINT('Ctrl Pts',(0.077316548567853,-0.599460146728784,
0.59510289473619));
#17088=CARTESIAN_POINT('Ctrl Pts',(0.0994608796208942,-0.577315815675743,
0.591804743154611));
#17089=CARTESIAN_POINT('Ctrl Pts',(0.109073016834181,-0.563290995658393,
0.590038488226116));
#17090=CARTESIAN_POINT('Ctrl Pts',(0.121843784097853,-0.532507913768158,
0.587534197873268));
#17091=CARTESIAN_POINT('Ctrl Pts',(0.125,-0.515745525063995,0.586834729715275));
#17092=CARTESIAN_POINT('Ctrl Pts',(0.125,-0.5,0.586834729715275));
#17093=CARTESIAN_POINT('',(-0.125,-0.5,0.));
#17094=CARTESIAN_POINT('Origin',(0.,0.,0.));
#17095=CARTESIAN_POINT('',(-0.6,-0.9,7.34788079488412E-17));
#17096=CARTESIAN_POINT('Origin',(0.,-0.9,0.));
#17097=CARTESIAN_POINT('',(-0.6,0.,7.34788079488412E-17));
#17098=CARTESIAN_POINT('',(-0.6,0.85,-7.34788079488412E-17));
#17099=CARTESIAN_POINT('',(-0.6,0.,7.34788079488412E-17));
#17100=CARTESIAN_POINT('Origin',(0.,0.85,0.));
#17101=CARTESIAN_POINT('Origin',(0.,-0.9,0.));
#17102=CARTESIAN_POINT('Origin',(0.,0.,0.));
#17103=CARTESIAN_POINT('',(-1.4,0.,1.71450551880629E-16));
#17104=CARTESIAN_POINT('Origin',(0.,0.,0.));
#17105=CARTESIAN_POINT('',(1.23958209161204,0.,0.143317017690053));
#17106=CARTESIAN_POINT('',(1.22320001975977,0.,0.246749348660852));
#17107=CARTESIAN_POINT('Origin',(1.21321664662686,0.,0.192154639568406));
#17108=CARTESIAN_POINT('',(1.20190105810224,0.,0.335465908756113));
#17109=CARTESIAN_POINT('Origin',(0.,0.,0.));
#17110=CARTESIAN_POINT('',(1.16954029537568,0.,0.435062095450087));
#17111=CARTESIAN_POINT('Origin',(1.1682203282434,0.,0.379577794185952));
#17112=CARTESIAN_POINT('',(1.13462523166105,0.,0.519354515801077));
#17113=CARTESIAN_POINT('Origin',(0.,0.,0.));
#17114=CARTESIAN_POINT('',(1.08708260743774,0.,0.612662169561029));
#17115=CARTESIAN_POINT('Origin',(1.0944585482776,0.,0.557654483764164));
#17116=CARTESIAN_POINT('',(1.0394111664111,0.,0.690454891028201));
#17117=CARTESIAN_POINT('Origin',(0.,0.,0.));
#17118=CARTESIAN_POINT('',(0.977857337884349,0.,0.775176467748211));
#17119=CARTESIAN_POINT('Origin',(0.993747566553533,0.,0.72199986920298));
#17120=CARTESIAN_POINT('',(0.918603348636233,0.,0.844553975349804));
#17121=CARTESIAN_POINT('Origin',(0.,0.,0.));
#17122=CARTESIAN_POINT('',(0.844553975349804,0.,0.918603348636233));
#17123=CARTESIAN_POINT('Origin',(0.86856722168183,0.,0.86856722168183));
#17124=CARTESIAN_POINT('',(0.775176467748211,0.,0.977857337884349));
#17125=CARTESIAN_POINT('Origin',(0.,0.,0.));
#17126=CARTESIAN_POINT('',(0.690454891028201,0.,1.0394111664111));
#17127=CARTESIAN_POINT('Origin',(0.721999869202979,0.,0.993747566553533));
#17128=CARTESIAN_POINT('',(0.612662169561028,0.,1.08708260743774));
#17129=CARTESIAN_POINT('Origin',(0.,0.,0.));
#17130=CARTESIAN_POINT('',(0.519354515801077,0.,1.13462523166105));
#17131=CARTESIAN_POINT('Origin',(0.557654483764164,0.,1.0944585482776));
#17132=CARTESIAN_POINT('',(0.435062095450087,0.,1.16954029537568));
#17133=CARTESIAN_POINT('Origin',(0.,0.,0.));
#17134=CARTESIAN_POINT('',(0.335465908756113,0.,1.20190105810224));
#17135=CARTESIAN_POINT('Origin',(0.379577794185951,0.,1.1682203282434));
#17136=CARTESIAN_POINT('',(0.246749348660851,0.,1.22320001975977));
#17137=CARTESIAN_POINT('Origin',(0.,0.,0.));
#17138=CARTESIAN_POINT('',(0.143317017690053,0.,1.23958209161204));
#17139=CARTESIAN_POINT('Origin',(0.192154639568406,0.,1.21321664662686));
#17140=CARTESIAN_POINT('',(0.0523608139934478,0.,1.24674050008925));
#17141=CARTESIAN_POINT('Origin',(0.,0.,0.));
#17142=CARTESIAN_POINT('',(-0.0523608139934483,0.,1.24674050008925));
#17143=CARTESIAN_POINT('Origin',(-2.25642313758905E-16,0.,1.22833954473516));
#17144=CARTESIAN_POINT('',(-0.143317017690053,0.,1.23958209161204));
#17145=CARTESIAN_POINT('Origin',(0.,0.,0.));
#17146=CARTESIAN_POINT('',(-0.246749348660852,0.,1.22320001975977));
#17147=CARTESIAN_POINT('Origin',(-0.192154639568406,0.,1.21321664662686));
#17148=CARTESIAN_POINT('',(-0.335465908756113,0.,1.20190105810224));
#17149=CARTESIAN_POINT('Origin',(0.,0.,0.));
#17150=CARTESIAN_POINT('',(-0.435062095450087,0.,1.16954029537568));
#17151=CARTESIAN_POINT('Origin',(-0.379577794185951,0.,1.1682203282434));
#17152=CARTESIAN_POINT('',(-0.519354515801077,0.,1.13462523166105));
#17153=CARTESIAN_POINT('Origin',(0.,0.,0.));
#17154=CARTESIAN_POINT('',(-0.612662169561029,0.,1.08708260743774));
#17155=CARTESIAN_POINT('Origin',(-0.557654483764164,0.,1.0944585482776));
#17156=CARTESIAN_POINT('',(-0.690454891028201,0.,1.0394111664111));
#17157=CARTESIAN_POINT('Origin',(0.,0.,0.));
#17158=CARTESIAN_POINT('',(-0.775176467748211,0.,0.977857337884349));
#17159=CARTESIAN_POINT('Origin',(-0.721999869202979,0.,0.993747566553533));
#17160=CARTESIAN_POINT('',(-0.844553975349804,0.,0.918603348636233));
#17161=CARTESIAN_POINT('Origin',(0.,0.,0.));
#17162=CARTESIAN_POINT('',(-0.918603348636233,0.,0.844553975349804));
#17163=CARTESIAN_POINT('Origin',(-0.86856722168183,0.,0.86856722168183));
#17164=CARTESIAN_POINT('',(-0.977857337884348,0.,0.775176467748211));
#17165=CARTESIAN_POINT('Origin',(0.,0.,0.));
#17166=CARTESIAN_POINT('',(-1.0394111664111,0.,0.690454891028201));
#17167=CARTESIAN_POINT('Origin',(-0.993747566553533,0.,0.721999869202979));
#17168=CARTESIAN_POINT('',(-1.08708260743774,0.,0.612662169561028));
#17169=CARTESIAN_POINT('Origin',(0.,0.,0.));
#17170=CARTESIAN_POINT('',(-1.13462523166105,0.,0.519354515801077));
#17171=CARTESIAN_POINT('Origin',(-1.0944585482776,0.,0.557654483764164));
#17172=CARTESIAN_POINT('',(-1.16954029537568,0.,0.435062095450087));
#17173=CARTESIAN_POINT('Origin',(0.,0.,0.));
#17174=CARTESIAN_POINT('',(-1.20190105810224,0.,0.335465908756113));
#17175=CARTESIAN_POINT('Origin',(-1.1682203282434,0.,0.379577794185951));
#17176=CARTESIAN_POINT('',(-1.22320001975977,0.,0.246749348660851));
#17177=CARTESIAN_POINT('Origin',(0.,0.,0.));
#17178=CARTESIAN_POINT('',(-1.23958209161204,0.,0.143317017690053));
#17179=CARTESIAN_POINT('Origin',(-1.21321664662686,0.,0.192154639568406));
#17180=CARTESIAN_POINT('',(-1.24674050008925,0.,0.0523608139934479));
#17181=CARTESIAN_POINT('Origin',(0.,0.,0.));
#17182=CARTESIAN_POINT('',(-1.24674050008925,0.,-0.0523608139934482));
#17183=CARTESIAN_POINT('Origin',(-1.22833954473516,0.,-1.50428209172603E-16));
#17184=CARTESIAN_POINT('',(-1.23958209161204,0.,-0.143317017690053));
#17185=CARTESIAN_POINT('Origin',(0.,0.,0.));
#17186=CARTESIAN_POINT('',(-1.22320001975977,0.,-0.246749348660852));
#17187=CARTESIAN_POINT('Origin',(-1.21321664662686,0.,-0.192154639568406));
#17188=CARTESIAN_POINT('',(-1.20190105810224,0.,-0.335465908756113));
#17189=CARTESIAN_POINT('Origin',(0.,0.,0.));
#17190=CARTESIAN_POINT('',(-1.16954029537568,0.,-0.435062095450087));
#17191=CARTESIAN_POINT('Origin',(-1.1682203282434,0.,-0.379577794185951));
#17192=CARTESIAN_POINT('',(-1.13462523166105,0.,-0.519354515801077));
#17193=CARTESIAN_POINT('Origin',(0.,0.,0.));
#17194=CARTESIAN_POINT('',(-1.08708260743774,0.,-0.612662169561029));
#17195=CARTESIAN_POINT('Origin',(-1.0944585482776,0.,-0.557654483764164));
#17196=CARTESIAN_POINT('',(-1.0394111664111,0.,-0.690454891028201));
#17197=CARTESIAN_POINT('Origin',(0.,0.,0.));
#17198=CARTESIAN_POINT('',(-0.977857337884349,0.,-0.775176467748211));
#17199=CARTESIAN_POINT('Origin',(-0.993747566553533,0.,-0.721999869202979));
#17200=CARTESIAN_POINT('',(-0.918603348636233,0.,-0.844553975349804));
#17201=CARTESIAN_POINT('Origin',(0.,0.,0.));
#17202=CARTESIAN_POINT('',(-0.844553975349804,0.,-0.918603348636233));
#17203=CARTESIAN_POINT('Origin',(-0.86856722168183,0.,-0.86856722168183));
#17204=CARTESIAN_POINT('',(-0.775176467748211,0.,-0.977857337884348));
#17205=CARTESIAN_POINT('Origin',(0.,0.,0.));
#17206=CARTESIAN_POINT('',(-0.690454891028201,0.,-1.0394111664111));
#17207=CARTESIAN_POINT('Origin',(-0.721999869202979,0.,-0.993747566553533));
#17208=CARTESIAN_POINT('',(-0.612662169561028,0.,-1.08708260743774));
#17209=CARTESIAN_POINT('Origin',(0.,0.,0.));
#17210=CARTESIAN_POINT('',(-0.519354515801077,0.,-1.13462523166105));
#17211=CARTESIAN_POINT('Origin',(-0.557654483764164,0.,-1.0944585482776));
#17212=CARTESIAN_POINT('',(-0.435062095450087,0.,-1.16954029537568));
#17213=CARTESIAN_POINT('Origin',(0.,0.,0.));
#17214=CARTESIAN_POINT('',(-0.335465908756113,0.,-1.20190105810224));
#17215=CARTESIAN_POINT('Origin',(-0.379577794185951,0.,-1.1682203282434));
#17216=CARTESIAN_POINT('',(-0.246749348660852,0.,-1.22320001975977));
#17217=CARTESIAN_POINT('Origin',(0.,0.,0.));
#17218=CARTESIAN_POINT('',(-0.143317017690053,0.,-1.23958209161204));
#17219=CARTESIAN_POINT('Origin',(-0.192154639568406,0.,-1.21321664662686));
#17220=CARTESIAN_POINT('',(-0.0523608139934479,0.,-1.24674050008925));
#17221=CARTESIAN_POINT('Origin',(0.,0.,0.));
#17222=CARTESIAN_POINT('',(0.0523608139934481,0.,-1.24674050008925));
#17223=CARTESIAN_POINT('Origin',(7.52141045863017E-17,0.,-1.22833954473516));
#17224=CARTESIAN_POINT('',(0.143317017690053,0.,-1.23958209161204));
#17225=CARTESIAN_POINT('Origin',(0.,0.,0.));
#17226=CARTESIAN_POINT('',(0.246749348660852,0.,-1.22320001975977));
#17227=CARTESIAN_POINT('Origin',(0.192154639568406,0.,-1.21321664662686));
#17228=CARTESIAN_POINT('',(0.335465908756113,0.,-1.20190105810224));
#17229=CARTESIAN_POINT('Origin',(0.,0.,0.));
#17230=CARTESIAN_POINT('',(0.435062095450087,0.,-1.16954029537568));
#17231=CARTESIAN_POINT('Origin',(0.379577794185951,0.,-1.1682203282434));
#17232=CARTESIAN_POINT('',(0.519354515801077,0.,-1.13462523166105));
#17233=CARTESIAN_POINT('Origin',(0.,0.,0.));
#17234=CARTESIAN_POINT('',(0.612662169561028,0.,-1.08708260743774));
#17235=CARTESIAN_POINT('Origin',(0.557654483764164,0.,-1.0944585482776));
#17236=CARTESIAN_POINT('',(0.690454891028201,0.,-1.0394111664111));
#17237=CARTESIAN_POINT('Origin',(0.,0.,0.));
#17238=CARTESIAN_POINT('',(0.775176467748211,0.,-0.977857337884349));
#17239=CARTESIAN_POINT('Origin',(0.721999869202979,0.,-0.993747566553533));
#17240=CARTESIAN_POINT('',(0.844553975349804,0.,-0.918603348636233));
#17241=CARTESIAN_POINT('Origin',(0.,0.,0.));
#17242=CARTESIAN_POINT('',(0.918603348636233,0.,-0.844553975349804));
#17243=CARTESIAN_POINT('Origin',(0.86856722168183,0.,-0.86856722168183));
#17244=CARTESIAN_POINT('',(0.977857337884349,0.,-0.775176467748211));
#17245=CARTESIAN_POINT('Origin',(0.,0.,0.));
#17246=CARTESIAN_POINT('',(1.0394111664111,0.,-0.690454891028201));
#17247=CARTESIAN_POINT('Origin',(0.993747566553533,0.,-0.721999869202979));
#17248=CARTESIAN_POINT('',(1.08708260743774,0.,-0.612662169561028));
#17249=CARTESIAN_POINT('Origin',(0.,0.,0.));
#17250=CARTESIAN_POINT('',(1.13462523166105,0.,-0.519354515801077));
#17251=CARTESIAN_POINT('Origin',(1.0944585482776,0.,-0.557654483764164));
#17252=CARTESIAN_POINT('',(1.16954029537568,0.,-0.43506209545009));
#17253=CARTESIAN_POINT('Origin',(0.,0.,0.));
#17254=CARTESIAN_POINT('',(1.20190105810224,0.,-0.33546590875611));
#17255=CARTESIAN_POINT('Origin',(1.1682203282434,0.,-0.379577794185951));
#17256=CARTESIAN_POINT('',(1.22320001975977,0.,-0.246749348660852));
#17257=CARTESIAN_POINT('Origin',(0.,0.,0.));
#17258=CARTESIAN_POINT('',(1.23958209161204,0.,-0.143317017690053));
#17259=CARTESIAN_POINT('Origin',(1.21321664662686,0.,-0.192154639568406));
#17260=CARTESIAN_POINT('',(1.24674050008925,0.,-0.052360813993451));
#17261=CARTESIAN_POINT('Origin',(0.,0.,0.));
#17262=CARTESIAN_POINT('',(1.24674050008925,0.,0.052360813993451));
#17263=CARTESIAN_POINT('Origin',(1.22833954473516,0.,0.));
#17264=CARTESIAN_POINT('Origin',(0.,0.,0.));
#17265=CARTESIAN_POINT('Origin',(0.,0.,0.));
#17266=CARTESIAN_POINT('',(-1.4,-0.1,1.71450551880629E-16));
#17267=CARTESIAN_POINT('Origin',(0.,-0.1,0.));
#17268=CARTESIAN_POINT('',(-1.4,0.,-1.71450551880629E-16));
#17269=CARTESIAN_POINT('Origin',(0.,-0.1,0.));
#17270=CARTESIAN_POINT('Origin',(0.,0.75,0.));
#17271=CARTESIAN_POINT('',(-1.4,0.75,1.71450551880629E-16));
#17272=CARTESIAN_POINT('Origin',(0.,0.75,0.));
#17273=CARTESIAN_POINT('',(1.22320001975977,0.75,0.246749348660852));
#17274=CARTESIAN_POINT('',(1.23958209161204,0.75,0.143317017690053));
#17275=CARTESIAN_POINT('Origin',(1.21321664662686,0.75,0.192154639568406));
#17276=CARTESIAN_POINT('',(1.24674050008925,0.75,0.052360813993448));
#17277=CARTESIAN_POINT('Origin',(0.,0.75,0.));
#17278=CARTESIAN_POINT('',(1.24674050008925,0.75,-0.052360813993448));
#17279=CARTESIAN_POINT('Origin',(1.22833954473516,0.75,0.));
#17280=CARTESIAN_POINT('',(1.23958209161204,0.75,-0.143317017690053));
#17281=CARTESIAN_POINT('Origin',(0.,0.75,0.));
#17282=CARTESIAN_POINT('',(1.22320001975977,0.75,-0.246749348660852));
#17283=CARTESIAN_POINT('Origin',(1.21321664662686,0.75,-0.192154639568406));
#17284=CARTESIAN_POINT('',(1.20190105810224,0.75,-0.335465908756113));
#17285=CARTESIAN_POINT('Origin',(0.,0.75,0.));
#17286=CARTESIAN_POINT('',(1.16954029537568,0.75,-0.435062095450087));
#17287=CARTESIAN_POINT('Origin',(1.1682203282434,0.75,-0.379577794185951));
#17288=CARTESIAN_POINT('',(1.13462523166105,0.75,-0.519354515801077));
#17289=CARTESIAN_POINT('Origin',(0.,0.75,0.));
#17290=CARTESIAN_POINT('',(1.08708260743774,0.75,-0.612662169561028));
#17291=CARTESIAN_POINT('Origin',(1.0944585482776,0.75,-0.557654483764164));
#17292=CARTESIAN_POINT('',(1.0394111664111,0.75,-0.690454891028201));
#17293=CARTESIAN_POINT('Origin',(0.,0.75,0.));
#17294=CARTESIAN_POINT('',(0.977857337884349,0.75,-0.775176467748211));
#17295=CARTESIAN_POINT('Origin',(0.993747566553533,0.75,-0.721999869202979));
#17296=CARTESIAN_POINT('',(0.918603348636233,0.75,-0.844553975349804));
#17297=CARTESIAN_POINT('Origin',(0.,0.75,0.));
#17298=CARTESIAN_POINT('',(0.844553975349804,0.75,-0.918603348636233));
#17299=CARTESIAN_POINT('Origin',(0.86856722168183,0.75,-0.86856722168183));
#17300=CARTESIAN_POINT('',(0.775176467748211,0.75,-0.977857337884349));
#17301=CARTESIAN_POINT('Origin',(0.,0.75,0.));
#17302=CARTESIAN_POINT('',(0.690454891028201,0.75,-1.0394111664111));
#17303=CARTESIAN_POINT('Origin',(0.721999869202979,0.75,-0.993747566553533));
#17304=CARTESIAN_POINT('',(0.612662169561028,0.75,-1.08708260743774));
#17305=CARTESIAN_POINT('Origin',(0.,0.75,0.));
#17306=CARTESIAN_POINT('',(0.519354515801077,0.75,-1.13462523166105));
#17307=CARTESIAN_POINT('Origin',(0.557654483764164,0.75,-1.0944585482776));
#17308=CARTESIAN_POINT('',(0.435062095450087,0.75,-1.16954029537568));
#17309=CARTESIAN_POINT('Origin',(0.,0.75,0.));
#17310=CARTESIAN_POINT('',(0.335465908756113,0.75,-1.20190105810224));
#17311=CARTESIAN_POINT('Origin',(0.379577794185951,0.75,-1.1682203282434));
#17312=CARTESIAN_POINT('',(0.246749348660852,0.75,-1.22320001975977));
#17313=CARTESIAN_POINT('Origin',(0.,0.75,0.));
#17314=CARTESIAN_POINT('',(0.143317017690053,0.75,-1.23958209161204));
#17315=CARTESIAN_POINT('Origin',(0.192154639568406,0.75,-1.21321664662686));
#17316=CARTESIAN_POINT('',(0.0523608139934481,0.75,-1.24674050008925));
#17317=CARTESIAN_POINT('Origin',(0.,0.75,0.));
#17318=CARTESIAN_POINT('',(-0.0523608139934479,0.75,-1.24674050008925));
#17319=CARTESIAN_POINT('Origin',(7.52141045863017E-17,0.75,-1.22833954473516));
#17320=CARTESIAN_POINT('',(-0.143317017690053,0.75,-1.23958209161204));
#17321=CARTESIAN_POINT('Origin',(0.,0.75,0.));
#17322=CARTESIAN_POINT('',(-0.246749348660852,0.75,-1.22320001975977));
#17323=CARTESIAN_POINT('Origin',(-0.192154639568406,0.75,-1.21321664662686));
#17324=CARTESIAN_POINT('',(-0.335465908756113,0.75,-1.20190105810224));
#17325=CARTESIAN_POINT('Origin',(0.,0.75,0.));
#17326=CARTESIAN_POINT('',(-0.435062095450087,0.75,-1.16954029537568));
#17327=CARTESIAN_POINT('Origin',(-0.379577794185951,0.75,-1.1682203282434));
#17328=CARTESIAN_POINT('',(-0.519354515801077,0.75,-1.13462523166105));
#17329=CARTESIAN_POINT('Origin',(0.,0.75,0.));
#17330=CARTESIAN_POINT('',(-0.612662169561028,0.75,-1.08708260743774));
#17331=CARTESIAN_POINT('Origin',(-0.557654483764164,0.75,-1.0944585482776));
#17332=CARTESIAN_POINT('',(-0.690454891028201,0.75,-1.0394111664111));
#17333=CARTESIAN_POINT('Origin',(0.,0.75,0.));
#17334=CARTESIAN_POINT('',(-0.775176467748211,0.75,-0.977857337884348));
#17335=CARTESIAN_POINT('Origin',(-0.721999869202979,0.75,-0.993747566553533));
#17336=CARTESIAN_POINT('',(-0.844553975349804,0.75,-0.918603348636233));
#17337=CARTESIAN_POINT('Origin',(0.,0.75,0.));
#17338=CARTESIAN_POINT('',(-0.918603348636233,0.75,-0.844553975349804));
#17339=CARTESIAN_POINT('Origin',(-0.86856722168183,0.75,-0.86856722168183));
#17340=CARTESIAN_POINT('',(-0.977857337884349,0.75,-0.775176467748211));
#17341=CARTESIAN_POINT('Origin',(0.,0.75,0.));
#17342=CARTESIAN_POINT('',(-1.0394111664111,0.75,-0.690454891028201));
#17343=CARTESIAN_POINT('Origin',(-0.993747566553533,0.75,-0.721999869202979));
#17344=CARTESIAN_POINT('',(-1.08708260743774,0.75,-0.612662169561029));
#17345=CARTESIAN_POINT('Origin',(0.,0.75,0.));
#17346=CARTESIAN_POINT('',(-1.13462523166105,0.75,-0.519354515801077));
#17347=CARTESIAN_POINT('Origin',(-1.0944585482776,0.75,-0.557654483764164));
#17348=CARTESIAN_POINT('',(-1.16954029537568,0.75,-0.435062095450087));
#17349=CARTESIAN_POINT('Origin',(0.,0.75,0.));
#17350=CARTESIAN_POINT('',(-1.20190105810224,0.75,-0.335465908756113));
#17351=CARTESIAN_POINT('Origin',(-1.1682203282434,0.75,-0.379577794185951));
#17352=CARTESIAN_POINT('',(-1.22320001975977,0.75,-0.246749348660852));
#17353=CARTESIAN_POINT('Origin',(0.,0.75,0.));
#17354=CARTESIAN_POINT('',(-1.23958209161204,0.75,-0.143317017690053));
#17355=CARTESIAN_POINT('Origin',(-1.21321664662686,0.75,-0.192154639568406));
#17356=CARTESIAN_POINT('',(-1.24674050008925,0.75,-0.0523608139934482));
#17357=CARTESIAN_POINT('Origin',(0.,0.75,0.));
#17358=CARTESIAN_POINT('',(-1.24674050008925,0.75,0.0523608139934479));
#17359=CARTESIAN_POINT('Origin',(-1.22833954473516,0.75,-1.50428209172603E-16));
#17360=CARTESIAN_POINT('',(-1.23958209161204,0.75,0.143317017690053));
#17361=CARTESIAN_POINT('Origin',(0.,0.75,0.));
#17362=CARTESIAN_POINT('',(-1.22320001975977,0.75,0.246749348660851));
#17363=CARTESIAN_POINT('Origin',(-1.21321664662686,0.75,0.192154639568406));
#17364=CARTESIAN_POINT('',(-1.20190105810224,0.75,0.335465908756113));
#17365=CARTESIAN_POINT('Origin',(0.,0.75,0.));
#17366=CARTESIAN_POINT('',(-1.16954029537568,0.75,0.435062095450087));
#17367=CARTESIAN_POINT('Origin',(-1.1682203282434,0.75,0.379577794185951));
#17368=CARTESIAN_POINT('',(-1.13462523166105,0.75,0.519354515801077));
#17369=CARTESIAN_POINT('Origin',(0.,0.75,0.));
#17370=CARTESIAN_POINT('',(-1.08708260743774,0.75,0.612662169561028));
#17371=CARTESIAN_POINT('Origin',(-1.0944585482776,0.75,0.557654483764164));
#17372=CARTESIAN_POINT('',(-1.0394111664111,0.75,0.690454891028201));
#17373=CARTESIAN_POINT('Origin',(0.,0.75,0.));
#17374=CARTESIAN_POINT('',(-0.977857337884348,0.75,0.775176467748211));
#17375=CARTESIAN_POINT('Origin',(-0.993747566553533,0.75,0.721999869202979));
#17376=CARTESIAN_POINT('',(-0.918603348636233,0.75,0.844553975349804));
#17377=CARTESIAN_POINT('Origin',(0.,0.75,0.));
#17378=CARTESIAN_POINT('',(-0.844553975349804,0.75,0.918603348636233));
#17379=CARTESIAN_POINT('Origin',(-0.86856722168183,0.75,0.86856722168183));
#17380=CARTESIAN_POINT('',(-0.775176467748211,0.75,0.977857337884349));
#17381=CARTESIAN_POINT('Origin',(0.,0.75,0.));
#17382=CARTESIAN_POINT('',(-0.690454891028201,0.75,1.0394111664111));
#17383=CARTESIAN_POINT('Origin',(-0.721999869202979,0.75,0.993747566553533));
#17384=CARTESIAN_POINT('',(-0.612662169561029,0.75,1.08708260743774));
#17385=CARTESIAN_POINT('Origin',(0.,0.75,0.));
#17386=CARTESIAN_POINT('',(-0.519354515801077,0.75,1.13462523166105));
#17387=CARTESIAN_POINT('Origin',(-0.557654483764164,0.75,1.0944585482776));
#17388=CARTESIAN_POINT('',(-0.435062095450087,0.75,1.16954029537568));
#17389=CARTESIAN_POINT('Origin',(0.,0.75,0.));
#17390=CARTESIAN_POINT('',(-0.335465908756113,0.75,1.20190105810224));
#17391=CARTESIAN_POINT('Origin',(-0.379577794185951,0.75,1.1682203282434));
#17392=CARTESIAN_POINT('',(-0.246749348660852,0.75,1.22320001975977));
#17393=CARTESIAN_POINT('Origin',(0.,0.75,0.));
#17394=CARTESIAN_POINT('',(-0.143317017690053,0.75,1.23958209161204));
#17395=CARTESIAN_POINT('Origin',(-0.192154639568406,0.75,1.21321664662686));
#17396=CARTESIAN_POINT('',(-0.0523608139934483,0.75,1.24674050008925));
#17397=CARTESIAN_POINT('Origin',(0.,0.75,0.));
#17398=CARTESIAN_POINT('',(0.0523608139934478,0.75,1.24674050008925));
#17399=CARTESIAN_POINT('Origin',(-2.25642313758905E-16,0.75,1.22833954473516));
#17400=CARTESIAN_POINT('',(0.143317017690053,0.75,1.23958209161204));
#17401=CARTESIAN_POINT('Origin',(0.,0.75,0.));
#17402=CARTESIAN_POINT('',(0.246749348660851,0.75,1.22320001975977));
#17403=CARTESIAN_POINT('Origin',(0.192154639568406,0.75,1.21321664662686));
#17404=CARTESIAN_POINT('',(0.335465908756113,0.75,1.20190105810224));
#17405=CARTESIAN_POINT('Origin',(0.,0.75,0.));
#17406=CARTESIAN_POINT('',(0.435062095450087,0.75,1.16954029537568));
#17407=CARTESIAN_POINT('Origin',(0.379577794185951,0.75,1.1682203282434));
#17408=CARTESIAN_POINT('',(0.519354515801077,0.75,1.13462523166105));
#17409=CARTESIAN_POINT('Origin',(0.,0.75,0.));
#17410=CARTESIAN_POINT('',(0.612662169561028,0.75,1.08708260743774));
#17411=CARTESIAN_POINT('Origin',(0.557654483764164,0.75,1.0944585482776));
#17412=CARTESIAN_POINT('',(0.690454891028201,0.75,1.0394111664111));
#17413=CARTESIAN_POINT('Origin',(0.,0.75,0.));
#17414=CARTESIAN_POINT('',(0.775176467748211,0.75,0.977857337884349));
#17415=CARTESIAN_POINT('Origin',(0.721999869202979,0.75,0.993747566553533));
#17416=CARTESIAN_POINT('',(0.844553975349804,0.75,0.918603348636233));
#17417=CARTESIAN_POINT('Origin',(0.,0.75,0.));
#17418=CARTESIAN_POINT('',(0.918603348636233,0.75,0.844553975349804));
#17419=CARTESIAN_POINT('Origin',(0.86856722168183,0.75,0.86856722168183));
#17420=CARTESIAN_POINT('',(0.977857337884349,0.75,0.775176467748211));
#17421=CARTESIAN_POINT('Origin',(0.,0.75,0.));
#17422=CARTESIAN_POINT('',(1.0394111664111,0.75,0.690454891028201));
#17423=CARTESIAN_POINT('Origin',(0.993747566553533,0.75,0.72199986920298));
#17424=CARTESIAN_POINT('',(1.08708260743774,0.75,0.612662169561029));
#17425=CARTESIAN_POINT('Origin',(0.,0.75,0.));
#17426=CARTESIAN_POINT('',(1.13462523166105,0.75,0.519354515801077));
#17427=CARTESIAN_POINT('Origin',(1.0944585482776,0.75,0.557654483764164));
#17428=CARTESIAN_POINT('',(1.16954029537568,0.75,0.435062095450087));
#17429=CARTESIAN_POINT('Origin',(0.,0.75,0.));
#17430=CARTESIAN_POINT('',(1.20190105810224,0.75,0.335465908756113));
#17431=CARTESIAN_POINT('Origin',(1.1682203282434,0.75,0.379577794185952));
#17432=CARTESIAN_POINT('Origin',(0.,0.75,0.));
#17433=CARTESIAN_POINT('Origin',(0.,0.75,0.));
#17434=CARTESIAN_POINT('',(-1.4,0.85,1.71450551880629E-16));
#17435=CARTESIAN_POINT('Origin',(0.,0.85,0.));
#17436=CARTESIAN_POINT('',(-1.4,0.75,1.71450551880629E-16));
#17437=CARTESIAN_POINT('Origin',(0.,0.85,0.));
#17438=CARTESIAN_POINT('Origin',(1.21321664662686,0.,0.192154639568406));
#17439=CARTESIAN_POINT('',(1.23958209161204,0.,0.14331701769005));
#17440=CARTESIAN_POINT('',(1.22320001975977,0.,0.246749348660855));
#17441=CARTESIAN_POINT('Origin',(0.,0.,0.));
#17442=CARTESIAN_POINT('',(1.20190105810224,0.,0.33546590875611));
#17443=CARTESIAN_POINT('Origin',(1.1682203282434,0.,0.379577794185952));
#17444=CARTESIAN_POINT('',(1.16954029537568,0.,0.43506209545009));
#17445=CARTESIAN_POINT('Origin',(0.,0.,0.));
#17446=CARTESIAN_POINT('',(1.13462523166105,0.,0.519354515801074));
#17447=CARTESIAN_POINT('Origin',(1.0944585482776,0.,0.557654483764164));
#17448=CARTESIAN_POINT('',(1.08708260743774,0.,0.612662169561031));
#17449=CARTESIAN_POINT('Origin',(0.,0.,0.));
#17450=CARTESIAN_POINT('',(1.03941116641111,0.,0.690454891028199));
#17451=CARTESIAN_POINT('Origin',(0.993747566553533,0.,0.72199986920298));
#17452=CARTESIAN_POINT('',(0.977857337884347,0.,0.775176467748214));
#17453=CARTESIAN_POINT('Origin',(0.,0.,0.));
#17454=CARTESIAN_POINT('',(0.918603348636235,0.,0.844553975349802));
#17455=CARTESIAN_POINT('Origin',(0.86856722168183,0.,0.86856722168183));
#17456=CARTESIAN_POINT('',(0.844553975349802,0.,0.918603348636235));
#17457=CARTESIAN_POINT('Origin',(0.,0.,0.));
#17458=CARTESIAN_POINT('',(0.775176467748213,0.,0.977857337884347));
#17459=CARTESIAN_POINT('Origin',(0.721999869202979,0.,0.993747566553533));
#17460=CARTESIAN_POINT('',(0.690454891028198,0.,1.03941116641111));
#17461=CARTESIAN_POINT('Origin',(0.,0.,0.));
#17462=CARTESIAN_POINT('',(0.612662169561031,0.,1.08708260743774));
#17463=CARTESIAN_POINT('Origin',(0.557654483764164,0.,1.0944585482776));
#17464=CARTESIAN_POINT('',(0.519354515801074,0.,1.13462523166105));
#17465=CARTESIAN_POINT('Origin',(0.,0.,0.));
#17466=CARTESIAN_POINT('',(0.43506209545009,0.,1.16954029537568));
#17467=CARTESIAN_POINT('Origin',(0.379577794185951,0.,1.1682203282434));
#17468=CARTESIAN_POINT('',(0.33546590875611,0.,1.20190105810224));
#17469=CARTESIAN_POINT('Origin',(0.,0.,0.));
#17470=CARTESIAN_POINT('',(0.246749348660854,0.,1.22320001975977));
#17471=CARTESIAN_POINT('Origin',(0.192154639568406,0.,1.21321664662686));
#17472=CARTESIAN_POINT('',(0.14331701769005,0.,1.23958209161204));
#17473=CARTESIAN_POINT('Origin',(0.,0.,0.));
#17474=CARTESIAN_POINT('',(0.0523608139934508,0.,1.24674050008925));
#17475=CARTESIAN_POINT('Origin',(-2.25642313758905E-16,0.,1.22833954473516));
#17476=CARTESIAN_POINT('',(-0.0523608139934513,0.,1.24674050008925));
#17477=CARTESIAN_POINT('Origin',(0.,0.,0.));
#17478=CARTESIAN_POINT('',(-0.14331701769005,0.,1.23958209161204));
#17479=CARTESIAN_POINT('Origin',(-0.192154639568406,0.,1.21321664662686));
#17480=CARTESIAN_POINT('',(-0.246749348660855,0.,1.22320001975977));
#17481=CARTESIAN_POINT('Origin',(0.,0.,0.));
#17482=CARTESIAN_POINT('',(-0.33546590875611,0.,1.20190105810224));
#17483=CARTESIAN_POINT('Origin',(-0.379577794185951,0.,1.1682203282434));
#17484=CARTESIAN_POINT('',(-0.43506209545009,0.,1.16954029537568));
#17485=CARTESIAN_POINT('Origin',(0.,0.,0.));
#17486=CARTESIAN_POINT('',(-0.519354515801074,0.,1.13462523166105));
#17487=CARTESIAN_POINT('Origin',(-0.557654483764164,0.,1.0944585482776));
#17488=CARTESIAN_POINT('',(-0.612662169561031,0.,1.08708260743774));
#17489=CARTESIAN_POINT('Origin',(0.,0.,0.));
#17490=CARTESIAN_POINT('',(-0.690454891028199,0.,1.03941116641111));
#17491=CARTESIAN_POINT('Origin',(-0.721999869202979,0.,0.993747566553533));
#17492=CARTESIAN_POINT('',(-0.775176467748213,0.,0.977857337884347));
#17493=CARTESIAN_POINT('Origin',(0.,0.,0.));
#17494=CARTESIAN_POINT('',(-0.844553975349802,0.,0.918603348636235));
#17495=CARTESIAN_POINT('Origin',(-0.86856722168183,0.,0.86856722168183));
#17496=CARTESIAN_POINT('',(-0.918603348636235,0.,0.844553975349802));
#17497=CARTESIAN_POINT('Origin',(0.,0.,0.));
#17498=CARTESIAN_POINT('',(-0.977857337884347,0.,0.775176467748213));
#17499=CARTESIAN_POINT('Origin',(-0.993747566553533,0.,0.721999869202979));
#17500=CARTESIAN_POINT('',(-1.03941116641111,0.,0.690454891028198));
#17501=CARTESIAN_POINT('Origin',(0.,0.,0.));
#17502=CARTESIAN_POINT('',(-1.08708260743774,0.,0.612662169561031));
#17503=CARTESIAN_POINT('Origin',(-1.0944585482776,0.,0.557654483764164));
#17504=CARTESIAN_POINT('',(-1.13462523166105,0.,0.519354515801074));
#17505=CARTESIAN_POINT('Origin',(0.,0.,0.));
#17506=CARTESIAN_POINT('',(-1.16954029537568,0.,0.43506209545009));
#17507=CARTESIAN_POINT('Origin',(-1.1682203282434,0.,0.379577794185951));
#17508=CARTESIAN_POINT('',(-1.20190105810224,0.,0.33546590875611));
#17509=CARTESIAN_POINT('Origin',(0.,0.,0.));
#17510=CARTESIAN_POINT('',(-1.22320001975977,0.,0.246749348660854));
#17511=CARTESIAN_POINT('Origin',(-1.21321664662686,0.,0.192154639568406));
#17512=CARTESIAN_POINT('',(-1.23958209161204,0.,0.14331701769005));
#17513=CARTESIAN_POINT('Origin',(0.,0.,0.));
#17514=CARTESIAN_POINT('',(-1.24674050008925,0.,0.0523608139934509));
#17515=CARTESIAN_POINT('Origin',(-1.22833954473516,0.,-1.50428209172603E-16));
#17516=CARTESIAN_POINT('',(-1.24674050008925,0.,-0.0523608139934512));
#17517=CARTESIAN_POINT('Origin',(0.,0.,0.));
#17518=CARTESIAN_POINT('',(-1.23958209161204,0.,-0.14331701769005));
#17519=CARTESIAN_POINT('Origin',(-1.21321664662686,0.,-0.192154639568406));
#17520=CARTESIAN_POINT('',(-1.22320001975977,0.,-0.246749348660855));
#17521=CARTESIAN_POINT('Origin',(0.,0.,0.));
#17522=CARTESIAN_POINT('',(-1.20190105810224,0.,-0.33546590875611));
#17523=CARTESIAN_POINT('Origin',(-1.1682203282434,0.,-0.379577794185951));
#17524=CARTESIAN_POINT('',(-1.16954029537568,0.,-0.43506209545009));
#17525=CARTESIAN_POINT('Origin',(0.,0.,0.));
#17526=CARTESIAN_POINT('',(-1.13462523166105,0.,-0.519354515801074));
#17527=CARTESIAN_POINT('Origin',(-1.0944585482776,0.,-0.557654483764164));
#17528=CARTESIAN_POINT('',(-1.08708260743774,0.,-0.612662169561031));
#17529=CARTESIAN_POINT('Origin',(0.,0.,0.));
#17530=CARTESIAN_POINT('',(-1.03941116641111,0.,-0.690454891028199));
#17531=CARTESIAN_POINT('Origin',(-0.993747566553533,0.,-0.721999869202979));
#17532=CARTESIAN_POINT('',(-0.977857337884347,0.,-0.775176467748213));
#17533=CARTESIAN_POINT('Origin',(0.,0.,0.));
#17534=CARTESIAN_POINT('',(-0.918603348636235,0.,-0.844553975349802));
#17535=CARTESIAN_POINT('Origin',(-0.86856722168183,0.,-0.86856722168183));
#17536=CARTESIAN_POINT('',(-0.844553975349802,0.,-0.918603348636235));
#17537=CARTESIAN_POINT('Origin',(0.,0.,0.));
#17538=CARTESIAN_POINT('',(-0.775176467748213,0.,-0.977857337884347));
#17539=CARTESIAN_POINT('Origin',(-0.721999869202979,0.,-0.993747566553533));
#17540=CARTESIAN_POINT('',(-0.690454891028198,0.,-1.03941116641111));
#17541=CARTESIAN_POINT('Origin',(0.,0.,0.));
#17542=CARTESIAN_POINT('',(-0.612662169561031,0.,-1.08708260743774));
#17543=CARTESIAN_POINT('Origin',(-0.557654483764164,0.,-1.0944585482776));
#17544=CARTESIAN_POINT('',(-0.519354515801074,0.,-1.13462523166105));
#17545=CARTESIAN_POINT('Origin',(0.,0.,0.));
#17546=CARTESIAN_POINT('',(-0.43506209545009,0.,-1.16954029537568));
#17547=CARTESIAN_POINT('Origin',(-0.379577794185951,0.,-1.1682203282434));
#17548=CARTESIAN_POINT('',(-0.33546590875611,0.,-1.20190105810224));
#17549=CARTESIAN_POINT('Origin',(0.,0.,0.));
#17550=CARTESIAN_POINT('',(-0.246749348660854,0.,-1.22320001975977));
#17551=CARTESIAN_POINT('Origin',(-0.192154639568406,0.,-1.21321664662686));
#17552=CARTESIAN_POINT('',(-0.14331701769005,0.,-1.23958209161204));
#17553=CARTESIAN_POINT('Origin',(0.,0.,0.));
#17554=CARTESIAN_POINT('',(-0.052360813993451,0.,-1.24674050008925));
#17555=CARTESIAN_POINT('Origin',(7.52141045863017E-17,0.,-1.22833954473516));
#17556=CARTESIAN_POINT('',(0.0523608139934511,0.,-1.24674050008925));
#17557=CARTESIAN_POINT('Origin',(0.,0.,0.));
#17558=CARTESIAN_POINT('',(0.14331701769005,0.,-1.23958209161204));
#17559=CARTESIAN_POINT('Origin',(0.192154639568406,0.,-1.21321664662686));
#17560=CARTESIAN_POINT('',(0.246749348660855,0.,-1.22320001975977));
#17561=CARTESIAN_POINT('Origin',(0.,0.,0.));
#17562=CARTESIAN_POINT('',(0.33546590875611,0.,-1.20190105810224));
#17563=CARTESIAN_POINT('Origin',(0.379577794185951,0.,-1.1682203282434));
#17564=CARTESIAN_POINT('',(0.43506209545009,0.,-1.16954029537568));
#17565=CARTESIAN_POINT('Origin',(0.,0.,0.));
#17566=CARTESIAN_POINT('',(0.519354515801074,0.,-1.13462523166105));
#17567=CARTESIAN_POINT('Origin',(0.557654483764164,0.,-1.0944585482776));
#17568=CARTESIAN_POINT('',(0.612662169561031,0.,-1.08708260743774));
#17569=CARTESIAN_POINT('Origin',(0.,0.,0.));
#17570=CARTESIAN_POINT('',(0.690454891028198,0.,-1.03941116641111));
#17571=CARTESIAN_POINT('Origin',(0.721999869202979,0.,-0.993747566553533));
#17572=CARTESIAN_POINT('',(0.775176467748213,0.,-0.977857337884347));
#17573=CARTESIAN_POINT('Origin',(0.,0.,0.));
#17574=CARTESIAN_POINT('',(0.844553975349802,0.,-0.918603348636235));
#17575=CARTESIAN_POINT('Origin',(0.86856722168183,0.,-0.86856722168183));
#17576=CARTESIAN_POINT('',(0.918603348636235,0.,-0.844553975349802));
#17577=CARTESIAN_POINT('Origin',(0.,0.,0.));
#17578=CARTESIAN_POINT('',(0.977857337884347,0.,-0.775176467748213));
#17579=CARTESIAN_POINT('Origin',(0.993747566553533,0.,-0.721999869202979));
#17580=CARTESIAN_POINT('',(1.03941116641111,0.,-0.690454891028198));
#17581=CARTESIAN_POINT('Origin',(0.,0.,0.));
#17582=CARTESIAN_POINT('',(1.08708260743774,0.,-0.612662169561031));
#17583=CARTESIAN_POINT('Origin',(1.0944585482776,0.,-0.557654483764164));
#17584=CARTESIAN_POINT('',(1.13462523166105,0.,-0.519354515801074));
#17585=CARTESIAN_POINT('Origin',(0.,0.,0.));
#17586=CARTESIAN_POINT('',(1.16954029537568,0.,-0.43506209545009));
#17587=CARTESIAN_POINT('Origin',(1.1682203282434,0.,-0.379577794185951));
#17588=CARTESIAN_POINT('',(1.20190105810224,0.,-0.33546590875611));
#17589=CARTESIAN_POINT('Origin',(0.,0.,0.));
#17590=CARTESIAN_POINT('',(1.22320001975977,0.,-0.246749348660855));
#17591=CARTESIAN_POINT('Origin',(1.21321664662686,0.,-0.192154639568406));
#17592=CARTESIAN_POINT('',(1.23958209161204,0.,-0.14331701769005));
#17593=CARTESIAN_POINT('Origin',(0.,0.,0.));
#17594=CARTESIAN_POINT('',(1.24674050008925,0.,0.052360813993451));
#17595=CARTESIAN_POINT('Origin',(1.22833954473516,0.,0.));
#17596=CARTESIAN_POINT('',(1.24674050008925,0.,-0.052360813993451));
#17597=CARTESIAN_POINT('Origin',(0.,0.,0.));
#17598=CARTESIAN_POINT('',(0.,0.,0.));
#17599=CARTESIAN_POINT('Origin',(0.3,0.4,0.));
#17600=CARTESIAN_POINT('',(-0.3,0.4,-3.67394039744206E-17));
#17601=CARTESIAN_POINT('Origin',(0.,0.4,0.));
#17602=CARTESIAN_POINT('Origin',(0.,0.375,0.));
#17603=CARTESIAN_POINT('',(-0.35,0.35,-4.28626379701573E-17));
#17604=CARTESIAN_POINT('Origin',(0.,0.35,0.));
#17605=CARTESIAN_POINT('',(-0.325,0.375,-3.9801020972289E-17));
#17606=CARTESIAN_POINT('Origin',(0.,0.19,0.));
#17607=CARTESIAN_POINT('',(-0.35,0.03,-4.28626379701574E-17));
#17608=CARTESIAN_POINT('Origin',(0.,0.03,0.));
#17609=CARTESIAN_POINT('',(-0.35,0.19,-4.28626379701574E-17));
#17610=CARTESIAN_POINT('Origin',(0.,0.0149999999999999,0.));
#17611=CARTESIAN_POINT('',(-0.32,-3.29597460435593E-17,-3.91886975727153E-17));
#17612=CARTESIAN_POINT('Origin',(0.,0.,0.));
#17613=CARTESIAN_POINT('',(-0.335,0.0149999999999999,-4.10256677714363E-17));
#17614=CARTESIAN_POINT('Origin',(0.22,0.,0.));
#17615=CARTESIAN_POINT('',(-0.22,-6.93889390390723E-18,-2.69422295812418E-17));
#17616=CARTESIAN_POINT('Origin',(0.,0.,0.));
#17617=CARTESIAN_POINT('Origin',(0.,-0.02,0.));
#17618=CARTESIAN_POINT('',(-0.1954,-0.0492,2.39295984553393E-17));
#17619=CARTESIAN_POINT('Origin',(0.,-0.0492,0.));
#17620=CARTESIAN_POINT('',(-0.21,-0.02,-2.57175827820944E-17));
#17621=CARTESIAN_POINT('Origin',(0.,-0.8,0.));
#17622=CARTESIAN_POINT('',(-0.1954,-1.5646,2.39295984553393E-17));
#17623=CARTESIAN_POINT('Origin',(0.,-1.5646,0.));
#17624=CARTESIAN_POINT('',(-0.1954,-0.8,-2.39295984553393E-17));
#17625=CARTESIAN_POINT('Origin',(0.,-1.58,0.));
#17626=CARTESIAN_POINT('',(-0.16,-1.6,-1.95943487863577E-17));
#17627=CARTESIAN_POINT('Origin',(0.,-1.6,0.));
#17628=CARTESIAN_POINT('',(-0.18,-1.58,-2.20436423846524E-17));
#17629=CARTESIAN_POINT('Origin',(0.,-1.6,0.));
#17630=CARTESIAN_POINT('Origin',(0.0866025403784439,-0.4,-0.15));
#17631=CARTESIAN_POINT('',(0.173205080756888,-0.4,0.));
#17632=CARTESIAN_POINT('',(0.0866025403784439,-0.4,-0.15));
#17633=CARTESIAN_POINT('',(0.173205080756888,-0.4,0.));
#17634=CARTESIAN_POINT('',(0.0866025403784439,-0.64,-0.15));
#17635=CARTESIAN_POINT('',(0.0866025403784439,-0.4,-0.15));
#17636=CARTESIAN_POINT('',(0.173205080756888,-0.64,0.));
#17637=CARTESIAN_POINT('',(0.173205080756888,-0.64,0.));
#17638=CARTESIAN_POINT('',(0.173205080756888,-0.4,0.));
#17639=CARTESIAN_POINT('Origin',(-0.0866025403784438,-0.4,-0.15));
#17640=CARTESIAN_POINT('',(-0.0866025403784438,-0.4,-0.15));
#17641=CARTESIAN_POINT('',(0.0866025403784439,-0.4,-0.15));
#17642=CARTESIAN_POINT('',(-0.0866025403784438,-0.64,-0.15));
#17643=CARTESIAN_POINT('',(-0.0866025403784438,-0.4,-0.15));
#17644=CARTESIAN_POINT('',(0.0866025403784439,-0.64,-0.15));
#17645=CARTESIAN_POINT('Origin',(-0.173205080756888,-0.4,-2.77555756156289E-17));
#17646=CARTESIAN_POINT('',(-0.173205080756888,-0.4,-2.12115047744981E-17));
#17647=CARTESIAN_POINT('',(-0.0866025403784438,-0.4,-0.15));
#17648=CARTESIAN_POINT('',(-0.173205080756888,-0.64,-2.77555756156289E-17));
#17649=CARTESIAN_POINT('',(-0.173205080756888,-0.4,-2.12115047744981E-17));
#17650=CARTESIAN_POINT('',(-0.0866025403784438,-0.64,-0.15));
#17651=CARTESIAN_POINT('Origin',(-0.0866025403784439,-0.4,0.15));
#17652=CARTESIAN_POINT('',(-0.0866025403784439,-0.4,0.15));
#17653=CARTESIAN_POINT('',(-0.173205080756888,-0.4,-2.12115047744981E-17));
#17654=CARTESIAN_POINT('',(-0.0866025403784439,-0.64,0.15));
#17655=CARTESIAN_POINT('',(-0.0866025403784439,-0.4,0.15));
#17656=CARTESIAN_POINT('',(-0.173205080756888,-0.64,-2.12115047744981E-17));
#17657=CARTESIAN_POINT('Origin',(0.0866025403784439,-0.4,0.15));
#17658=CARTESIAN_POINT('',(0.0866025403784439,-0.4,0.15));
#17659=CARTESIAN_POINT('',(-0.0866025403784439,-0.4,0.15));
#17660=CARTESIAN_POINT('',(0.0866025403784439,-0.64,0.15));
#17661=CARTESIAN_POINT('',(0.0866025403784439,-0.4,0.15));
#17662=CARTESIAN_POINT('',(-0.0866025403784439,-0.64,0.15));
#17663=CARTESIAN_POINT('Origin',(0.173205080756888,-0.4,0.));
#17664=CARTESIAN_POINT('',(0.0866025403784439,-0.4,0.15));
#17665=CARTESIAN_POINT('',(0.0866025403784439,-0.64,0.15));
#17666=CARTESIAN_POINT('Origin',(0.,-0.4,-2.77555756156289E-17));
#17667=CARTESIAN_POINT('Origin',(0.,-0.64,-2.77555756156289E-17));
#17668=CARTESIAN_POINT('',(0.,0.,0.));
#17669=CARTESIAN_POINT('',(0.,0.,0.));
#17670=CARTESIAN_POINT('',(0.,0.,0.));
#17671=CARTESIAN_POINT('',(0.,0.,0.));
#17672=CARTESIAN_POINT('',(0.,0.,0.));
#17673=CARTESIAN_POINT('',(0.,0.,0.));
#17674=CARTESIAN_POINT('',(0.,0.,0.));
#17675=CARTESIAN_POINT('',(0.,0.,0.));
#17676=CARTESIAN_POINT('',(0.,0.,0.));
#17677=CARTESIAN_POINT('',(0.,0.,0.));
#17678=CARTESIAN_POINT('',(0.,0.,0.));
#17679=CARTESIAN_POINT('',(0.,0.,0.));
#17680=CARTESIAN_POINT('',(0.,0.,0.));
#17681=CARTESIAN_POINT('',(0.,0.,0.));
#17682=CARTESIAN_POINT('',(0.,0.,0.));
#17683=CARTESIAN_POINT('',(0.,0.,0.));
#17684=CARTESIAN_POINT('',(-2.8,-1.,0.8));
#17685=CARTESIAN_POINT('',(-2.8,1.,0.8));
#17686=CARTESIAN_POINT('',(2.8,-1.,0.8));
#17687=CARTESIAN_POINT('',(2.8,1.,0.8));
#17688=CARTESIAN_POINT('',(0.,-0.9,7.));
#17689=CARTESIAN_POINT('',(0.,0.9,7.));
#17690=CARTESIAN_POINT('',(1.34350288425444,-2.1,8.34350288425444));
#17691=CARTESIAN_POINT('',(-1.34350288425444,-2.1,8.34350288425444));
#17692=CARTESIAN_POINT('',(-1.34350288425444,-2.1,5.65649711574556));
#17693=CARTESIAN_POINT('',(1.34350288425444,-2.1,5.65649711574556));
#17694=CARTESIAN_POINT('',(1.34350288425444,2.1,8.34350288425444));
#17695=CARTESIAN_POINT('',(-1.34350288425444,2.1,8.34350288425444));
#17696=CARTESIAN_POINT('',(-1.34350288425444,2.1,5.65649711574556));
#17697=CARTESIAN_POINT('',(1.34350288425444,2.1,5.65649711574556));
#17698=CARTESIAN_POINT('',(4.17091003018116,-1.,0.8));
#17699=CARTESIAN_POINT('',(4.17091003018116,1.,0.8));
#17700=CARTESIAN_POINT('',(9.77091003018116,-1.,0.8));
#17701=CARTESIAN_POINT('',(9.77091003018116,1.,0.8));
#17702=CARTESIAN_POINT('',(6.97091003018116,-0.9,7.));
#17703=CARTESIAN_POINT('',(6.97091003018116,0.9,7.));
#17704=CARTESIAN_POINT('',(8.38512359255425,-2.1,8.4142135623731));
#17705=CARTESIAN_POINT('',(5.55669646780806,-2.1,8.4142135623731));
#17706=CARTESIAN_POINT('',(5.55669646780806,-2.1,5.58578643762691));
#17707=CARTESIAN_POINT('',(8.38512359255425,-2.1,5.58578643762691));
#17708=CARTESIAN_POINT('',(8.38512359255425,2.1,8.4142135623731));
#17709=CARTESIAN_POINT('',(5.55669646780806,2.1,8.4142135623731));
#17710=CARTESIAN_POINT('',(5.55669646780806,2.1,5.58578643762691));
#17711=CARTESIAN_POINT('',(8.38512359255425,2.1,5.58578643762691));
#17712=CARTESIAN_POINT('',(0.,0.,0.));
#17713=CARTESIAN_POINT('',(0.,0.,0.));
#17714=CARTESIAN_POINT('',(0.,0.,0.));
#17715=CARTESIAN_POINT('',(0.,0.,0.));
#17716=CARTESIAN_POINT('',(0.,0.,0.));
#17717=CARTESIAN_POINT('',(0.,0.,0.));
#17718=CARTESIAN_POINT('',(0.,-3.5,7.));
#17719=CARTESIAN_POINT('',(0.,-5.2,7.));
#17720=CARTESIAN_POINT('',(0.,0.,0.));
#17721=CARTESIAN_POINT('',(0.,0.,0.));
#17722=CARTESIAN_POINT('',(0.,0.,0.));
#17723=CARTESIAN_POINT('',(0.,0.,0.));
#17724=CARTESIAN_POINT('',(0.,0.,0.));
#17725=CARTESIAN_POINT('',(0.,0.,0.));
#17726=CARTESIAN_POINT('',(6.97091003018116,-3.5,7.));
#17727=CARTESIAN_POINT('',(6.97091003018116,-5.2,7.));
#17728=CARTESIAN_POINT('',(0.,0.,0.));
#17729=CARTESIAN_POINT('',(0.,0.,0.));
#17730=CARTESIAN_POINT('',(0.,0.,0.));
#17731=UNCERTAINTY_MEASURE_WITH_UNIT(LENGTH_MEASURE(0.001),#17831,
'DISTANCE_ACCURACY_VALUE',
'Maximum model space distance between geometric entities at asserted c
onnectivities');
#17732=UNCERTAINTY_MEASURE_WITH_UNIT(LENGTH_MEASURE(0.001),#17831,
'DISTANCE_ACCURACY_VALUE',
'Maximum model space distance between geometric entities at asserted c
onnectivities');
#17733=UNCERTAINTY_MEASURE_WITH_UNIT(LENGTH_MEASURE(0.001),#17831,
'DISTANCE_ACCURACY_VALUE',
'Maximum model space distance between geometric entities at asserted c
onnectivities');
#17734=UNCERTAINTY_MEASURE_WITH_UNIT(LENGTH_MEASURE(0.001),#17831,
'DISTANCE_ACCURACY_VALUE',
'Maximum model space distance between geometric entities at asserted c
onnectivities');
#17735=UNCERTAINTY_MEASURE_WITH_UNIT(LENGTH_MEASURE(0.001),#17831,
'DISTANCE_ACCURACY_VALUE',
'Maximum model space distance between geometric entities at asserted c
onnectivities');
#17736=UNCERTAINTY_MEASURE_WITH_UNIT(LENGTH_MEASURE(0.001),#17831,
'DISTANCE_ACCURACY_VALUE',
'Maximum model space distance between geometric entities at asserted c
onnectivities');
#17737=UNCERTAINTY_MEASURE_WITH_UNIT(LENGTH_MEASURE(0.001),#17831,
'DISTANCE_ACCURACY_VALUE',
'Maximum model space distance between geometric entities at asserted c
onnectivities');
#17738=UNCERTAINTY_MEASURE_WITH_UNIT(LENGTH_MEASURE(0.001),#17831,
'DISTANCE_ACCURACY_VALUE',
'Maximum model space distance between geometric entities at asserted c
onnectivities');
#17739=UNCERTAINTY_MEASURE_WITH_UNIT(LENGTH_MEASURE(0.001),#17831,
'DISTANCE_ACCURACY_VALUE',
'Maximum model space distance between geometric entities at asserted c
onnectivities');
#17740=UNCERTAINTY_MEASURE_WITH_UNIT(LENGTH_MEASURE(0.001),#17831,
'DISTANCE_ACCURACY_VALUE',
'Maximum model space distance between geometric entities at asserted c
onnectivities');
#17741=UNCERTAINTY_MEASURE_WITH_UNIT(LENGTH_MEASURE(0.001),#17831,
'DISTANCE_ACCURACY_VALUE',
'Maximum model space distance between geometric entities at asserted c
onnectivities');
#17742=UNCERTAINTY_MEASURE_WITH_UNIT(LENGTH_MEASURE(0.001),#17831,
'DISTANCE_ACCURACY_VALUE',
'Maximum model space distance between geometric entities at asserted c
onnectivities');
#17743=UNCERTAINTY_MEASURE_WITH_UNIT(LENGTH_MEASURE(0.001),#17831,
'DISTANCE_ACCURACY_VALUE',
'Maximum model space distance between geometric entities at asserted c
onnectivities');
#17744=UNCERTAINTY_MEASURE_WITH_UNIT(LENGTH_MEASURE(0.001),#17831,
'DISTANCE_ACCURACY_VALUE',
'Maximum model space distance between geometric entities at asserted c
onnectivities');
#17745=UNCERTAINTY_MEASURE_WITH_UNIT(LENGTH_MEASURE(0.001),#17831,
'DISTANCE_ACCURACY_VALUE',
'Maximum model space distance between geometric entities at asserted c
onnectivities');
#17746=UNCERTAINTY_MEASURE_WITH_UNIT(LENGTH_MEASURE(0.001),#17831,
'DISTANCE_ACCURACY_VALUE',
'Maximum model space distance between geometric entities at asserted c
onnectivities');
#17747=UNCERTAINTY_MEASURE_WITH_UNIT(LENGTH_MEASURE(0.001),#17831,
'DISTANCE_ACCURACY_VALUE',
'Maximum model space distance between geometric entities at asserted c
onnectivities');
#17748=UNCERTAINTY_MEASURE_WITH_UNIT(LENGTH_MEASURE(0.001),#17831,
'DISTANCE_ACCURACY_VALUE',
'Maximum model space distance between geometric entities at asserted c
onnectivities');
#17749=UNCERTAINTY_MEASURE_WITH_UNIT(LENGTH_MEASURE(0.001),#17831,
'DISTANCE_ACCURACY_VALUE',
'Maximum model space distance between geometric entities at asserted c
onnectivities');
#17750=UNCERTAINTY_MEASURE_WITH_UNIT(LENGTH_MEASURE(0.001),#17831,
'DISTANCE_ACCURACY_VALUE',
'Maximum model space distance between geometric entities at asserted c
onnectivities');
#17751=UNCERTAINTY_MEASURE_WITH_UNIT(LENGTH_MEASURE(0.001),#17831,
'DISTANCE_ACCURACY_VALUE',
'Maximum model space distance between geometric entities at asserted c
onnectivities');
#17752=UNCERTAINTY_MEASURE_WITH_UNIT(LENGTH_MEASURE(0.001),#17831,
'DISTANCE_ACCURACY_VALUE',
'Maximum model space distance between geometric entities at asserted c
onnectivities');
#17753=UNCERTAINTY_MEASURE_WITH_UNIT(LENGTH_MEASURE(0.001),#17831,
'DISTANCE_ACCURACY_VALUE',
'Maximum model space distance between geometric entities at asserted c
onnectivities');
#17754=UNCERTAINTY_MEASURE_WITH_UNIT(LENGTH_MEASURE(0.001),#17831,
'DISTANCE_ACCURACY_VALUE',
'Maximum model space distance between geometric entities at asserted c
onnectivities');
#17755=UNCERTAINTY_MEASURE_WITH_UNIT(LENGTH_MEASURE(0.001),#17831,
'DISTANCE_ACCURACY_VALUE',
'Maximum model space distance between geometric entities at asserted c
onnectivities');
#17756=UNCERTAINTY_MEASURE_WITH_UNIT(LENGTH_MEASURE(0.001),#17831,
'DISTANCE_ACCURACY_VALUE',
'Maximum model space distance between geometric entities at asserted c
onnectivities');
#17757=UNCERTAINTY_MEASURE_WITH_UNIT(LENGTH_MEASURE(0.001),#17831,
'DISTANCE_ACCURACY_VALUE',
'Maximum model space distance between geometric entities at asserted c
onnectivities');
#17758=UNCERTAINTY_MEASURE_WITH_UNIT(LENGTH_MEASURE(0.001),#17831,
'DISTANCE_ACCURACY_VALUE',
'Maximum model space distance between geometric entities at asserted c
onnectivities');
#17759=UNCERTAINTY_MEASURE_WITH_UNIT(LENGTH_MEASURE(0.001),#17831,
'DISTANCE_ACCURACY_VALUE',
'Maximum model space distance between geometric entities at asserted c
onnectivities');
#17760=UNCERTAINTY_MEASURE_WITH_UNIT(LENGTH_MEASURE(0.001),#17831,
'DISTANCE_ACCURACY_VALUE',
'Maximum model space distance between geometric entities at asserted c
onnectivities');
#17761=UNCERTAINTY_MEASURE_WITH_UNIT(LENGTH_MEASURE(0.001),#17831,
'DISTANCE_ACCURACY_VALUE',
'Maximum model space distance between geometric entities at asserted c
onnectivities');
#17762=UNCERTAINTY_MEASURE_WITH_UNIT(LENGTH_MEASURE(0.001),#17831,
'DISTANCE_ACCURACY_VALUE',
'Maximum model space distance between geometric entities at asserted c
onnectivities');
#17763=UNCERTAINTY_MEASURE_WITH_UNIT(LENGTH_MEASURE(0.001),#17831,
'DISTANCE_ACCURACY_VALUE',
'Maximum model space distance between geometric entities at asserted c
onnectivities');
#17764=UNCERTAINTY_MEASURE_WITH_UNIT(LENGTH_MEASURE(0.001),#17831,
'DISTANCE_ACCURACY_VALUE',
'Maximum model space distance between geometric entities at asserted c
onnectivities');
#17765=UNCERTAINTY_MEASURE_WITH_UNIT(LENGTH_MEASURE(0.001),#17831,
'DISTANCE_ACCURACY_VALUE',
'Maximum model space distance between geometric entities at asserted c
onnectivities');
#17766=UNCERTAINTY_MEASURE_WITH_UNIT(LENGTH_MEASURE(0.001),#17831,
'DISTANCE_ACCURACY_VALUE',
'Maximum model space distance between geometric entities at asserted c
onnectivities');
#17767=UNCERTAINTY_MEASURE_WITH_UNIT(LENGTH_MEASURE(0.001),#17831,
'DISTANCE_ACCURACY_VALUE',
'Maximum model space distance between geometric entities at asserted c
onnectivities');
#17768=UNCERTAINTY_MEASURE_WITH_UNIT(LENGTH_MEASURE(0.001),#17831,
'DISTANCE_ACCURACY_VALUE',
'Maximum model space distance between geometric entities at asserted c
onnectivities');
#17769=UNCERTAINTY_MEASURE_WITH_UNIT(LENGTH_MEASURE(0.001),#17831,
'DISTANCE_ACCURACY_VALUE',
'Maximum model space distance between geometric entities at asserted c
onnectivities');
#17770=UNCERTAINTY_MEASURE_WITH_UNIT(LENGTH_MEASURE(0.001),#17831,
'DISTANCE_ACCURACY_VALUE',
'Maximum model space distance between geometric entities at asserted c
onnectivities');
#17771=UNCERTAINTY_MEASURE_WITH_UNIT(LENGTH_MEASURE(0.001),#17831,
'DISTANCE_ACCURACY_VALUE',
'Maximum model space distance between geometric entities at asserted c
onnectivities');
#17772=UNCERTAINTY_MEASURE_WITH_UNIT(LENGTH_MEASURE(0.001),#17831,
'DISTANCE_ACCURACY_VALUE',
'Maximum model space distance between geometric entities at asserted c
onnectivities');
#17773=UNCERTAINTY_MEASURE_WITH_UNIT(LENGTH_MEASURE(0.001),#17831,
'DISTANCE_ACCURACY_VALUE',
'Maximum model space distance between geometric entities at asserted c
onnectivities');
#17774=UNCERTAINTY_MEASURE_WITH_UNIT(LENGTH_MEASURE(0.001),#17831,
'DISTANCE_ACCURACY_VALUE',
'Maximum model space distance between geometric entities at asserted c
onnectivities');
#17775=UNCERTAINTY_MEASURE_WITH_UNIT(LENGTH_MEASURE(0.001),#17831,
'DISTANCE_ACCURACY_VALUE',
'Maximum model space distance between geometric entities at asserted c
onnectivities');
#17776=UNCERTAINTY_MEASURE_WITH_UNIT(LENGTH_MEASURE(0.001),#17831,
'DISTANCE_ACCURACY_VALUE',
'Maximum model space distance between geometric entities at asserted c
onnectivities');
#17777=UNCERTAINTY_MEASURE_WITH_UNIT(LENGTH_MEASURE(0.001),#17831,
'DISTANCE_ACCURACY_VALUE',
'Maximum model space distance between geometric entities at asserted c
onnectivities');
#17778=UNCERTAINTY_MEASURE_WITH_UNIT(LENGTH_MEASURE(0.001),#17831,
'DISTANCE_ACCURACY_VALUE',
'Maximum model space distance between geometric entities at asserted c
onnectivities');
#17779=UNCERTAINTY_MEASURE_WITH_UNIT(LENGTH_MEASURE(0.001),#17831,
'DISTANCE_ACCURACY_VALUE',
'Maximum model space distance between geometric entities at asserted c
onnectivities');
#17780=UNCERTAINTY_MEASURE_WITH_UNIT(LENGTH_MEASURE(0.001),#17831,
'DISTANCE_ACCURACY_VALUE',
'Maximum model space distance between geometric entities at asserted c
onnectivities');
#17781=(
GEOMETRIC_REPRESENTATION_CONTEXT(3)
GLOBAL_UNCERTAINTY_ASSIGNED_CONTEXT((#17731))
GLOBAL_UNIT_ASSIGNED_CONTEXT((#17831,#17833,#17834))
REPRESENTATION_CONTEXT('','3D')
);
#17782=(
GEOMETRIC_REPRESENTATION_CONTEXT(3)
GLOBAL_UNCERTAINTY_ASSIGNED_CONTEXT((#17732))
GLOBAL_UNIT_ASSIGNED_CONTEXT((#17831,#17833,#17834))
REPRESENTATION_CONTEXT('','3D')
);
#17783=(
GEOMETRIC_REPRESENTATION_CONTEXT(3)
GLOBAL_UNCERTAINTY_ASSIGNED_CONTEXT((#17733))
GLOBAL_UNIT_ASSIGNED_CONTEXT((#17831,#17833,#17834))
REPRESENTATION_CONTEXT('','3D')
);
#17784=(
GEOMETRIC_REPRESENTATION_CONTEXT(3)
GLOBAL_UNCERTAINTY_ASSIGNED_CONTEXT((#17734))
GLOBAL_UNIT_ASSIGNED_CONTEXT((#17831,#17833,#17834))
REPRESENTATION_CONTEXT('','3D')
);
#17785=(
GEOMETRIC_REPRESENTATION_CONTEXT(3)
GLOBAL_UNCERTAINTY_ASSIGNED_CONTEXT((#17735))
GLOBAL_UNIT_ASSIGNED_CONTEXT((#17831,#17833,#17834))
REPRESENTATION_CONTEXT('','3D')
);
#17786=(
GEOMETRIC_REPRESENTATION_CONTEXT(3)
GLOBAL_UNCERTAINTY_ASSIGNED_CONTEXT((#17736))
GLOBAL_UNIT_ASSIGNED_CONTEXT((#17831,#17833,#17834))
REPRESENTATION_CONTEXT('','3D')
);
#17787=(
GEOMETRIC_REPRESENTATION_CONTEXT(3)
GLOBAL_UNCERTAINTY_ASSIGNED_CONTEXT((#17737))
GLOBAL_UNIT_ASSIGNED_CONTEXT((#17831,#17833,#17834))
REPRESENTATION_CONTEXT('','3D')
);
#17788=(
GEOMETRIC_REPRESENTATION_CONTEXT(3)
GLOBAL_UNCERTAINTY_ASSIGNED_CONTEXT((#17738))
GLOBAL_UNIT_ASSIGNED_CONTEXT((#17831,#17833,#17834))
REPRESENTATION_CONTEXT('','3D')
);
#17789=(
GEOMETRIC_REPRESENTATION_CONTEXT(3)
GLOBAL_UNCERTAINTY_ASSIGNED_CONTEXT((#17739))
GLOBAL_UNIT_ASSIGNED_CONTEXT((#17831,#17833,#17834))
REPRESENTATION_CONTEXT('','3D')
);
#17790=(
GEOMETRIC_REPRESENTATION_CONTEXT(3)
GLOBAL_UNCERTAINTY_ASSIGNED_CONTEXT((#17740))
GLOBAL_UNIT_ASSIGNED_CONTEXT((#17831,#17833,#17834))
REPRESENTATION_CONTEXT('','3D')
);
#17791=(
GEOMETRIC_REPRESENTATION_CONTEXT(3)
GLOBAL_UNCERTAINTY_ASSIGNED_CONTEXT((#17741))
GLOBAL_UNIT_ASSIGNED_CONTEXT((#17831,#17833,#17834))
REPRESENTATION_CONTEXT('','3D')
);
#17792=(
GEOMETRIC_REPRESENTATION_CONTEXT(3)
GLOBAL_UNCERTAINTY_ASSIGNED_CONTEXT((#17742))
GLOBAL_UNIT_ASSIGNED_CONTEXT((#17831,#17833,#17834))
REPRESENTATION_CONTEXT('','3D')
);
#17793=(
GEOMETRIC_REPRESENTATION_CONTEXT(3)
GLOBAL_UNCERTAINTY_ASSIGNED_CONTEXT((#17743))
GLOBAL_UNIT_ASSIGNED_CONTEXT((#17831,#17833,#17834))
REPRESENTATION_CONTEXT('','3D')
);
#17794=(
GEOMETRIC_REPRESENTATION_CONTEXT(3)
GLOBAL_UNCERTAINTY_ASSIGNED_CONTEXT((#17744))
GLOBAL_UNIT_ASSIGNED_CONTEXT((#17831,#17833,#17834))
REPRESENTATION_CONTEXT('','3D')
);
#17795=(
GEOMETRIC_REPRESENTATION_CONTEXT(3)
GLOBAL_UNCERTAINTY_ASSIGNED_CONTEXT((#17745))
GLOBAL_UNIT_ASSIGNED_CONTEXT((#17831,#17833,#17834))
REPRESENTATION_CONTEXT('','3D')
);
#17796=(
GEOMETRIC_REPRESENTATION_CONTEXT(3)
GLOBAL_UNCERTAINTY_ASSIGNED_CONTEXT((#17746))
GLOBAL_UNIT_ASSIGNED_CONTEXT((#17831,#17833,#17834))
REPRESENTATION_CONTEXT('','3D')
);
#17797=(
GEOMETRIC_REPRESENTATION_CONTEXT(3)
GLOBAL_UNCERTAINTY_ASSIGNED_CONTEXT((#17747))
GLOBAL_UNIT_ASSIGNED_CONTEXT((#17831,#17833,#17834))
REPRESENTATION_CONTEXT('','3D')
);
#17798=(
GEOMETRIC_REPRESENTATION_CONTEXT(3)
GLOBAL_UNCERTAINTY_ASSIGNED_CONTEXT((#17748))
GLOBAL_UNIT_ASSIGNED_CONTEXT((#17831,#17833,#17834))
REPRESENTATION_CONTEXT('','3D')
);
#17799=(
GEOMETRIC_REPRESENTATION_CONTEXT(3)
GLOBAL_UNCERTAINTY_ASSIGNED_CONTEXT((#17749))
GLOBAL_UNIT_ASSIGNED_CONTEXT((#17831,#17833,#17834))
REPRESENTATION_CONTEXT('','3D')
);
#17800=(
GEOMETRIC_REPRESENTATION_CONTEXT(3)
GLOBAL_UNCERTAINTY_ASSIGNED_CONTEXT((#17750))
GLOBAL_UNIT_ASSIGNED_CONTEXT((#17831,#17833,#17834))
REPRESENTATION_CONTEXT('','3D')
);
#17801=(
GEOMETRIC_REPRESENTATION_CONTEXT(3)
GLOBAL_UNCERTAINTY_ASSIGNED_CONTEXT((#17751))
GLOBAL_UNIT_ASSIGNED_CONTEXT((#17831,#17833,#17834))
REPRESENTATION_CONTEXT('','3D')
);
#17802=(
GEOMETRIC_REPRESENTATION_CONTEXT(3)
GLOBAL_UNCERTAINTY_ASSIGNED_CONTEXT((#17752))
GLOBAL_UNIT_ASSIGNED_CONTEXT((#17831,#17833,#17834))
REPRESENTATION_CONTEXT('','3D')
);
#17803=(
GEOMETRIC_REPRESENTATION_CONTEXT(3)
GLOBAL_UNCERTAINTY_ASSIGNED_CONTEXT((#17753))
GLOBAL_UNIT_ASSIGNED_CONTEXT((#17831,#17833,#17834))
REPRESENTATION_CONTEXT('','3D')
);
#17804=(
GEOMETRIC_REPRESENTATION_CONTEXT(3)
GLOBAL_UNCERTAINTY_ASSIGNED_CONTEXT((#17754))
GLOBAL_UNIT_ASSIGNED_CONTEXT((#17831,#17833,#17834))
REPRESENTATION_CONTEXT('','3D')
);
#17805=(
GEOMETRIC_REPRESENTATION_CONTEXT(3)
GLOBAL_UNCERTAINTY_ASSIGNED_CONTEXT((#17755))
GLOBAL_UNIT_ASSIGNED_CONTEXT((#17831,#17833,#17834))
REPRESENTATION_CONTEXT('','3D')
);
#17806=(
GEOMETRIC_REPRESENTATION_CONTEXT(3)
GLOBAL_UNCERTAINTY_ASSIGNED_CONTEXT((#17756))
GLOBAL_UNIT_ASSIGNED_CONTEXT((#17831,#17833,#17834))
REPRESENTATION_CONTEXT('','3D')
);
#17807=(
GEOMETRIC_REPRESENTATION_CONTEXT(3)
GLOBAL_UNCERTAINTY_ASSIGNED_CONTEXT((#17757))
GLOBAL_UNIT_ASSIGNED_CONTEXT((#17831,#17833,#17834))
REPRESENTATION_CONTEXT('','3D')
);
#17808=(
GEOMETRIC_REPRESENTATION_CONTEXT(3)
GLOBAL_UNCERTAINTY_ASSIGNED_CONTEXT((#17758))
GLOBAL_UNIT_ASSIGNED_CONTEXT((#17831,#17833,#17834))
REPRESENTATION_CONTEXT('','3D')
);
#17809=(
GEOMETRIC_REPRESENTATION_CONTEXT(3)
GLOBAL_UNCERTAINTY_ASSIGNED_CONTEXT((#17759))
GLOBAL_UNIT_ASSIGNED_CONTEXT((#17831,#17833,#17834))
REPRESENTATION_CONTEXT('','3D')
);
#17810=(
GEOMETRIC_REPRESENTATION_CONTEXT(3)
GLOBAL_UNCERTAINTY_ASSIGNED_CONTEXT((#17760))
GLOBAL_UNIT_ASSIGNED_CONTEXT((#17831,#17833,#17834))
REPRESENTATION_CONTEXT('','3D')
);
#17811=(
GEOMETRIC_REPRESENTATION_CONTEXT(3)
GLOBAL_UNCERTAINTY_ASSIGNED_CONTEXT((#17761))
GLOBAL_UNIT_ASSIGNED_CONTEXT((#17831,#17833,#17834))
REPRESENTATION_CONTEXT('','3D')
);
#17812=(
GEOMETRIC_REPRESENTATION_CONTEXT(3)
GLOBAL_UNCERTAINTY_ASSIGNED_CONTEXT((#17762))
GLOBAL_UNIT_ASSIGNED_CONTEXT((#17831,#17833,#17834))
REPRESENTATION_CONTEXT('','3D')
);
#17813=(
GEOMETRIC_REPRESENTATION_CONTEXT(3)
GLOBAL_UNCERTAINTY_ASSIGNED_CONTEXT((#17763))
GLOBAL_UNIT_ASSIGNED_CONTEXT((#17831,#17833,#17834))
REPRESENTATION_CONTEXT('','3D')
);
#17814=(
GEOMETRIC_REPRESENTATION_CONTEXT(3)
GLOBAL_UNCERTAINTY_ASSIGNED_CONTEXT((#17764))
GLOBAL_UNIT_ASSIGNED_CONTEXT((#17831,#17833,#17834))
REPRESENTATION_CONTEXT('','3D')
);
#17815=(
GEOMETRIC_REPRESENTATION_CONTEXT(3)
GLOBAL_UNCERTAINTY_ASSIGNED_CONTEXT((#17765))
GLOBAL_UNIT_ASSIGNED_CONTEXT((#17831,#17833,#17834))
REPRESENTATION_CONTEXT('','3D')
);
#17816=(
GEOMETRIC_REPRESENTATION_CONTEXT(3)
GLOBAL_UNCERTAINTY_ASSIGNED_CONTEXT((#17766))
GLOBAL_UNIT_ASSIGNED_CONTEXT((#17831,#17833,#17834))
REPRESENTATION_CONTEXT('','3D')
);
#17817=(
GEOMETRIC_REPRESENTATION_CONTEXT(3)
GLOBAL_UNCERTAINTY_ASSIGNED_CONTEXT((#17767))
GLOBAL_UNIT_ASSIGNED_CONTEXT((#17831,#17833,#17834))
REPRESENTATION_CONTEXT('','3D')
);
#17818=(
GEOMETRIC_REPRESENTATION_CONTEXT(3)
GLOBAL_UNCERTAINTY_ASSIGNED_CONTEXT((#17768))
GLOBAL_UNIT_ASSIGNED_CONTEXT((#17831,#17833,#17834))
REPRESENTATION_CONTEXT('','3D')
);
#17819=(
GEOMETRIC_REPRESENTATION_CONTEXT(3)
GLOBAL_UNCERTAINTY_ASSIGNED_CONTEXT((#17769))
GLOBAL_UNIT_ASSIGNED_CONTEXT((#17831,#17833,#17834))
REPRESENTATION_CONTEXT('','3D')
);
#17820=(
GEOMETRIC_REPRESENTATION_CONTEXT(3)
GLOBAL_UNCERTAINTY_ASSIGNED_CONTEXT((#17770))
GLOBAL_UNIT_ASSIGNED_CONTEXT((#17831,#17833,#17834))
REPRESENTATION_CONTEXT('','3D')
);
#17821=(
GEOMETRIC_REPRESENTATION_CONTEXT(3)
GLOBAL_UNCERTAINTY_ASSIGNED_CONTEXT((#17771))
GLOBAL_UNIT_ASSIGNED_CONTEXT((#17831,#17833,#17834))
REPRESENTATION_CONTEXT('','3D')
);
#17822=(
GEOMETRIC_REPRESENTATION_CONTEXT(3)
GLOBAL_UNCERTAINTY_ASSIGNED_CONTEXT((#17772))
GLOBAL_UNIT_ASSIGNED_CONTEXT((#17831,#17833,#17834))
REPRESENTATION_CONTEXT('','3D')
);
#17823=(
GEOMETRIC_REPRESENTATION_CONTEXT(3)
GLOBAL_UNCERTAINTY_ASSIGNED_CONTEXT((#17773))
GLOBAL_UNIT_ASSIGNED_CONTEXT((#17831,#17833,#17834))
REPRESENTATION_CONTEXT('','3D')
);
#17824=(
GEOMETRIC_REPRESENTATION_CONTEXT(3)
GLOBAL_UNCERTAINTY_ASSIGNED_CONTEXT((#17774))
GLOBAL_UNIT_ASSIGNED_CONTEXT((#17831,#17833,#17834))
REPRESENTATION_CONTEXT('','3D')
);
#17825=(
GEOMETRIC_REPRESENTATION_CONTEXT(3)
GLOBAL_UNCERTAINTY_ASSIGNED_CONTEXT((#17775))
GLOBAL_UNIT_ASSIGNED_CONTEXT((#17831,#17833,#17834))
REPRESENTATION_CONTEXT('','3D')
);
#17826=(
GEOMETRIC_REPRESENTATION_CONTEXT(3)
GLOBAL_UNCERTAINTY_ASSIGNED_CONTEXT((#17776))
GLOBAL_UNIT_ASSIGNED_CONTEXT((#17831,#17833,#17834))
REPRESENTATION_CONTEXT('','3D')
);
#17827=(
GEOMETRIC_REPRESENTATION_CONTEXT(3)
GLOBAL_UNCERTAINTY_ASSIGNED_CONTEXT((#17777))
GLOBAL_UNIT_ASSIGNED_CONTEXT((#17831,#17833,#17834))
REPRESENTATION_CONTEXT('','3D')
);
#17828=(
GEOMETRIC_REPRESENTATION_CONTEXT(3)
GLOBAL_UNCERTAINTY_ASSIGNED_CONTEXT((#17778))
GLOBAL_UNIT_ASSIGNED_CONTEXT((#17831,#17833,#17834))
REPRESENTATION_CONTEXT('','3D')
);
#17829=(
GEOMETRIC_REPRESENTATION_CONTEXT(3)
GLOBAL_UNCERTAINTY_ASSIGNED_CONTEXT((#17779))
GLOBAL_UNIT_ASSIGNED_CONTEXT((#17831,#17833,#17834))
REPRESENTATION_CONTEXT('','3D')
);
#17830=(
GEOMETRIC_REPRESENTATION_CONTEXT(3)
GLOBAL_UNCERTAINTY_ASSIGNED_CONTEXT((#17780))
GLOBAL_UNIT_ASSIGNED_CONTEXT((#17831,#17833,#17834))
REPRESENTATION_CONTEXT('','3D')
);
#17831=(
LENGTH_UNIT()
NAMED_UNIT(*)
SI_UNIT(.CENTI.,.METRE.)
);
#17832=(
LENGTH_UNIT()
NAMED_UNIT(*)
SI_UNIT($,.METRE.)
);
#17833=(
NAMED_UNIT(*)
PLANE_ANGLE_UNIT()
SI_UNIT($,.RADIAN.)
);
#17834=(
NAMED_UNIT(*)
SI_UNIT($,.STERADIAN.)
SOLID_ANGLE_UNIT()
);
#17835=SHAPE_DEFINITION_REPRESENTATION(#17884,#18006);
#17836=SHAPE_DEFINITION_REPRESENTATION(#17885,#18007);
#17837=SHAPE_DEFINITION_REPRESENTATION(#17886,#18008);
#17838=SHAPE_DEFINITION_REPRESENTATION(#17887,#18009);
#17839=SHAPE_DEFINITION_REPRESENTATION(#17888,#18010);
#17840=SHAPE_DEFINITION_REPRESENTATION(#17889,#18011);
#17841=SHAPE_DEFINITION_REPRESENTATION(#17890,#18012);
#17842=SHAPE_DEFINITION_REPRESENTATION(#17891,#18013);
#17843=SHAPE_DEFINITION_REPRESENTATION(#17892,#18014);
#17844=SHAPE_DEFINITION_REPRESENTATION(#17893,#18015);
#17845=SHAPE_DEFINITION_REPRESENTATION(#17894,#18016);
#17846=SHAPE_DEFINITION_REPRESENTATION(#17895,#18017);
#17847=SHAPE_DEFINITION_REPRESENTATION(#17896,#18018);
#17848=SHAPE_DEFINITION_REPRESENTATION(#17897,#18019);
#17849=SHAPE_DEFINITION_REPRESENTATION(#17898,#18020);
#17850=SHAPE_DEFINITION_REPRESENTATION(#17899,#18021);
#17851=SHAPE_DEFINITION_REPRESENTATION(#17900,#18022);
#17852=SHAPE_DEFINITION_REPRESENTATION(#17901,#18023);
#17853=SHAPE_DEFINITION_REPRESENTATION(#17902,#18024);
#17854=SHAPE_DEFINITION_REPRESENTATION(#17903,#18025);
#17855=SHAPE_DEFINITION_REPRESENTATION(#17904,#18026);
#17856=SHAPE_DEFINITION_REPRESENTATION(#17905,#18027);
#17857=SHAPE_DEFINITION_REPRESENTATION(#17906,#18028);
#17858=SHAPE_DEFINITION_REPRESENTATION(#17907,#18029);
#17859=SHAPE_DEFINITION_REPRESENTATION(#17913,#18030);
#17860=SHAPE_DEFINITION_REPRESENTATION(#17914,#18031);
#17861=SHAPE_DEFINITION_REPRESENTATION(#17915,#18032);
#17862=SHAPE_DEFINITION_REPRESENTATION(#17916,#18033);
#17863=SHAPE_DEFINITION_REPRESENTATION(#17917,#18034);
#17864=SHAPE_DEFINITION_REPRESENTATION(#17918,#18035);
#17865=SHAPE_DEFINITION_REPRESENTATION(#17919,#18036);
#17866=SHAPE_DEFINITION_REPRESENTATION(#17925,#18037);
#17867=SHAPE_DEFINITION_REPRESENTATION(#17926,#18038);
#17868=SHAPE_DEFINITION_REPRESENTATION(#17927,#18039);
#17869=SHAPE_DEFINITION_REPRESENTATION(#17928,#18040);
#17870=SHAPE_DEFINITION_REPRESENTATION(#17929,#18041);
#17871=SHAPE_DEFINITION_REPRESENTATION(#17930,#18042);
#17872=SHAPE_DEFINITION_REPRESENTATION(#17931,#18043);
#17873=SHAPE_DEFINITION_REPRESENTATION(#17932,#18044);
#17874=SHAPE_DEFINITION_REPRESENTATION(#17933,#18045);
#17875=SHAPE_DEFINITION_REPRESENTATION(#17934,#18046);
#17876=SHAPE_DEFINITION_REPRESENTATION(#17935,#18047);
#17877=SHAPE_DEFINITION_REPRESENTATION(#17936,#18048);
#17878=SHAPE_DEFINITION_REPRESENTATION(#17937,#18049);
#17879=SHAPE_DEFINITION_REPRESENTATION(#17938,#18050);
#17880=SHAPE_DEFINITION_REPRESENTATION(#17939,#18051);
#17881=SHAPE_DEFINITION_REPRESENTATION(#17940,#18052);
#17882=SHAPE_DEFINITION_REPRESENTATION(#17941,#18053);
#17883=SHAPE_DEFINITION_REPRESENTATION(#17942,#18054);
#17884=PRODUCT_DEFINITION_SHAPE('',$,#18056);
#17885=PRODUCT_DEFINITION_SHAPE('',$,#18057);
#17886=PRODUCT_DEFINITION_SHAPE('',$,#18058);
#17887=PRODUCT_DEFINITION_SHAPE('',$,#18059);
#17888=PRODUCT_DEFINITION_SHAPE('',$,#18060);
#17889=PRODUCT_DEFINITION_SHAPE('',$,#18061);
#17890=PRODUCT_DEFINITION_SHAPE('',$,#18062);
#17891=PRODUCT_DEFINITION_SHAPE('',$,#18063);
#17892=PRODUCT_DEFINITION_SHAPE('',$,#18064);
#17893=PRODUCT_DEFINITION_SHAPE('',$,#18065);
#17894=PRODUCT_DEFINITION_SHAPE('',$,#18066);
#17895=PRODUCT_DEFINITION_SHAPE('',$,#18067);
#17896=PRODUCT_DEFINITION_SHAPE('',$,#18068);
#17897=PRODUCT_DEFINITION_SHAPE('',$,#18069);
#17898=PRODUCT_DEFINITION_SHAPE('',$,#18070);
#17899=PRODUCT_DEFINITION_SHAPE('',$,#18071);
#17900=PRODUCT_DEFINITION_SHAPE('',$,#18072);
#17901=PRODUCT_DEFINITION_SHAPE('',$,#18073);
#17902=PRODUCT_DEFINITION_SHAPE('',$,#18074);
#17903=PRODUCT_DEFINITION_SHAPE('',$,#18075);
#17904=PRODUCT_DEFINITION_SHAPE('',$,#18076);
#17905=PRODUCT_DEFINITION_SHAPE('',$,#18077);
#17906=PRODUCT_DEFINITION_SHAPE('',$,#18078);
#17907=PRODUCT_DEFINITION_SHAPE('',$,#18079);
#17908=PRODUCT_DEFINITION_SHAPE($,$,#236);
#17909=PRODUCT_DEFINITION_SHAPE($,$,#237);
#17910=PRODUCT_DEFINITION_SHAPE($,$,#238);
#17911=PRODUCT_DEFINITION_SHAPE($,$,#239);
#17912=PRODUCT_DEFINITION_SHAPE($,$,#240);
#17913=PRODUCT_DEFINITION_SHAPE('',$,#18080);
#17914=PRODUCT_DEFINITION_SHAPE('',$,#18081);
#17915=PRODUCT_DEFINITION_SHAPE('',$,#18082);
#17916=PRODUCT_DEFINITION_SHAPE('',$,#18083);
#17917=PRODUCT_DEFINITION_SHAPE('',$,#18084);
#17918=PRODUCT_DEFINITION_SHAPE('',$,#18085);
#17919=PRODUCT_DEFINITION_SHAPE('',$,#18086);
#17920=PRODUCT_DEFINITION_SHAPE($,$,#241);
#17921=PRODUCT_DEFINITION_SHAPE($,$,#242);
#17922=PRODUCT_DEFINITION_SHAPE($,$,#243);
#17923=PRODUCT_DEFINITION_SHAPE($,$,#244);
#17924=PRODUCT_DEFINITION_SHAPE($,$,#245);
#17925=PRODUCT_DEFINITION_SHAPE('',$,#18087);
#17926=PRODUCT_DEFINITION_SHAPE('',$,#18088);
#17927=PRODUCT_DEFINITION_SHAPE('',$,#18089);
#17928=PRODUCT_DEFINITION_SHAPE('',$,#18090);
#17929=PRODUCT_DEFINITION_SHAPE('',$,#18091);
#17930=PRODUCT_DEFINITION_SHAPE('',$,#18092);
#17931=PRODUCT_DEFINITION_SHAPE('',$,#18093);
#17932=PRODUCT_DEFINITION_SHAPE('',$,#18094);
#17933=PRODUCT_DEFINITION_SHAPE('',$,#18095);
#17934=PRODUCT_DEFINITION_SHAPE('',$,#18096);
#17935=PRODUCT_DEFINITION_SHAPE('',$,#18097);
#17936=PRODUCT_DEFINITION_SHAPE('',$,#18098);
#17937=PRODUCT_DEFINITION_SHAPE('',$,#18099);
#17938=PRODUCT_DEFINITION_SHAPE('',$,#18100);
#17939=PRODUCT_DEFINITION_SHAPE('',$,#18101);
#17940=PRODUCT_DEFINITION_SHAPE('',$,#18102);
#17941=PRODUCT_DEFINITION_SHAPE('',$,#18103);
#17942=PRODUCT_DEFINITION_SHAPE('',$,#18104);
#17943=PRODUCT_DEFINITION_SHAPE($,$,#246);
#17944=PRODUCT_DEFINITION_SHAPE($,$,#247);
#17945=PRODUCT_DEFINITION_SHAPE($,$,#248);
#17946=PRODUCT_DEFINITION_SHAPE($,$,#249);
#17947=PRODUCT_DEFINITION_SHAPE($,$,#250);
#17948=PRODUCT_DEFINITION_SHAPE($,$,#251);
#17949=PRODUCT_DEFINITION_SHAPE($,$,#252);
#17950=PRODUCT_DEFINITION_SHAPE($,$,#253);
#17951=PRODUCT_DEFINITION_SHAPE($,$,#254);
#17952=PRODUCT_DEFINITION_SHAPE($,$,#255);
#17953=PRODUCT_DEFINITION_SHAPE($,$,#256);
#17954=PRODUCT_DEFINITION_SHAPE($,$,#257);
#17955=PRODUCT_DEFINITION_SHAPE($,$,#258);
#17956=PRODUCT_DEFINITION_SHAPE($,$,#259);
#17957=PRODUCT_DEFINITION_SHAPE($,$,#260);
#17958=PRODUCT_DEFINITION_SHAPE($,$,#261);
#17959=PRODUCT_DEFINITION_SHAPE($,$,#262);
#17960=PRODUCT_DEFINITION_SHAPE($,$,#263);
#17961=PRODUCT_DEFINITION_SHAPE($,$,#264);
#17962=PRODUCT_DEFINITION_SHAPE($,$,#265);
#17963=PRODUCT_DEFINITION_SHAPE($,$,#266);
#17964=PRODUCT_DEFINITION_SHAPE($,$,#267);
#17965=PRODUCT_DEFINITION_SHAPE($,$,#268);
#17966=PRODUCT_DEFINITION_SHAPE($,$,#269);
#17967=PRODUCT_DEFINITION_SHAPE($,$,#270);
#17968=PRODUCT_DEFINITION_SHAPE($,$,#271);
#17969=PRODUCT_DEFINITION_SHAPE($,$,#272);
#17970=PRODUCT_DEFINITION_SHAPE($,$,#273);
#17971=PRODUCT_DEFINITION_SHAPE($,$,#274);
#17972=PRODUCT_DEFINITION_SHAPE($,$,#275);
#17973=PRODUCT_DEFINITION_SHAPE($,$,#276);
#17974=PRODUCT_DEFINITION_SHAPE($,$,#277);
#17975=PRODUCT_DEFINITION_SHAPE($,$,#278);
#17976=PRODUCT_DEFINITION_SHAPE($,$,#279);
#17977=PRODUCT_DEFINITION_SHAPE($,$,#280);
#17978=PRODUCT_DEFINITION_SHAPE($,$,#281);
#17979=PRODUCT_DEFINITION_SHAPE($,$,#282);
#17980=PRODUCT_DEFINITION_SHAPE($,$,#283);
#17981=PRODUCT_DEFINITION_SHAPE($,$,#284);
#17982=PRODUCT_DEFINITION_SHAPE($,$,#285);
#17983=PRODUCT_DEFINITION_SHAPE($,$,#286);
#17984=PRODUCT_DEFINITION_SHAPE($,$,#287);
#17985=PRODUCT_DEFINITION_SHAPE($,$,#288);
#17986=PRODUCT_DEFINITION_SHAPE($,$,#289);
#17987=PRODUCT_DEFINITION_SHAPE($,$,#290);
#17988=PRODUCT_DEFINITION_SHAPE($,$,#291);
#17989=PRODUCT_DEFINITION_SHAPE($,$,#292);
#17990=PRODUCT_DEFINITION_SHAPE($,$,#293);
#17991=PRODUCT_DEFINITION_SHAPE($,$,#294);
#17992=PRODUCT_DEFINITION_SHAPE($,$,#295);
#17993=PRODUCT_DEFINITION_SHAPE($,$,#296);
#17994=PRODUCT_DEFINITION_SHAPE($,$,#297);
#17995=PRODUCT_DEFINITION_SHAPE($,$,#298);
#17996=PRODUCT_DEFINITION_SHAPE($,$,#299);
#17997=PRODUCT_DEFINITION_SHAPE($,$,#300);
#17998=PRODUCT_DEFINITION_SHAPE($,$,#301);
#17999=PRODUCT_DEFINITION_SHAPE($,$,#302);
#18000=PRODUCT_DEFINITION_SHAPE($,$,#303);
#18001=PRODUCT_DEFINITION_SHAPE($,$,#304);
#18002=PRODUCT_DEFINITION_SHAPE($,$,#305);
#18003=PRODUCT_DEFINITION_SHAPE($,$,#306);
#18004=PRODUCT_DEFINITION_SHAPE($,$,#307);
#18005=PRODUCT_DEFINITION_SHAPE($,$,#308);
#18006=SHAPE_REPRESENTATION('',(#9516,#10806,#10807,#10808),#17781);
#18007=SHAPE_REPRESENTATION('',(#9517,#10746,#10747,#10748,#10749,#10750,
#10751,#10752,#10753,#10754,#10755,#10756,#10757,#10758,#10759,#10760,#10761,
#10762,#10763,#10764,#10765,#10766,#10767,#10768,#10769,#10770,#10771,#10772,
#10773,#10774,#10775,#10776,#10777,#10778,#10779,#10780,#10781,#10782,#10783,
#10784,#10785,#10786,#10787,#10788,#10789),#17782);
#18008=SHAPE_REPRESENTATION('',(#9518),#17783);
#18009=SHAPE_REPRESENTATION('',(#9577),#17784);
#18010=SHAPE_REPRESENTATION('',(#9584),#17785);
#18011=SHAPE_REPRESENTATION('',(#9591),#17786);
#18012=SHAPE_REPRESENTATION('',(#9629),#17787);
#18013=SHAPE_REPRESENTATION('',(#9638),#17788);
#18014=SHAPE_REPRESENTATION('',(#9672),#17789);
#18015=SHAPE_REPRESENTATION('',(#9706),#17790);
#18016=SHAPE_REPRESENTATION('',(#9744),#17791);
#18017=SHAPE_REPRESENTATION('',(#9753),#17792);
#18018=SHAPE_REPRESENTATION('',(#9762),#17793);
#18019=SHAPE_REPRESENTATION('',(#9771),#17794);
#18020=SHAPE_REPRESENTATION('',(#9780),#17795);
#18021=SHAPE_REPRESENTATION('',(#9789),#17796);
#18022=SHAPE_REPRESENTATION('',(#9823),#17797);
#18023=SHAPE_REPRESENTATION('',(#9857),#17798);
#18024=SHAPE_REPRESENTATION('',(#9876,#10005,#10006,#10007,#10008,#10009),
#17799);
#18025=SHAPE_REPRESENTATION('',(#9877),#17800);
#18026=SHAPE_REPRESENTATION('',(#9897),#17801);
#18027=SHAPE_REPRESENTATION('',(#9917),#17802);
#18028=SHAPE_REPRESENTATION('',(#9934),#17803);
#18029=SHAPE_REPRESENTATION('',(#9988),#17804);
#18030=SHAPE_REPRESENTATION('',(#10010),#17805);
#18031=SHAPE_REPRESENTATION('',(#10040,#10163,#10164,#10165,#10166,#10167),
#17806);
#18032=SHAPE_REPRESENTATION('',(#10041),#17807);
#18033=SHAPE_REPRESENTATION('',(#10061),#17808);
#18034=SHAPE_REPRESENTATION('',(#10081),#17809);
#18035=SHAPE_REPRESENTATION('',(#10096),#17810);
#18036=SHAPE_REPRESENTATION('',(#10146),#17811);
#18037=SHAPE_REPRESENTATION('',(#10168),#17812);
#18038=SHAPE_REPRESENTATION('',(#10192,#10790,#10791,#10792,#10793,#10794,
#10795,#10796,#10797),#17813);
#18039=SHAPE_REPRESENTATION('',(#10193),#17814);
#18040=SHAPE_REPRESENTATION('',(#10215),#17815);
#18041=SHAPE_REPRESENTATION('',(#10228),#17816);
#18042=SHAPE_REPRESENTATION('',(#10237),#17817);
#18043=SHAPE_REPRESENTATION('',(#10243),#17818);
#18044=SHAPE_REPRESENTATION('',(#10249),#17819);
#18045=SHAPE_REPRESENTATION('',(#10258),#17820);
#18046=SHAPE_REPRESENTATION('',(#10400,#10798,#10799,#10800,#10801,#10802,
#10803,#10804,#10805),#17821);
#18047=SHAPE_REPRESENTATION('',(#10401),#17822);
#18048=SHAPE_REPRESENTATION('',(#10419),#17823);
#18049=SHAPE_REPRESENTATION('',(#10428),#17824);
#18050=SHAPE_REPRESENTATION('',(#10437),#17825);
#18051=SHAPE_REPRESENTATION('',(#10443),#17826);
#18052=SHAPE_REPRESENTATION('',(#10449),#17827);
#18053=SHAPE_REPRESENTATION('',(#10458),#17828);
#18054=SHAPE_REPRESENTATION('',(#10720),#17829);
#18055=PRODUCT_DEFINITION_CONTEXT('part definition',#18204,'design');
#18056=PRODUCT_DEFINITION(
'PAT-104','PAT-104',#18105,
#18055);
#18057=PRODUCT_DEFINITION('Bearing base and belt envelope',
'Bearing base and belt envelope',#18106,#18055);
#18058=PRODUCT_DEFINITION('Base','Base',#18107,#18055);
#18059=PRODUCT_DEFINITION('Foot','Foot',#18108,#18055);
#18060=PRODUCT_DEFINITION('Foot (1)','Foot (1)',#18109,#18055);
#18061=PRODUCT_DEFINITION('Fixed bearing block','Fixed bearing block',#18110,
#18055);
#18062=PRODUCT_DEFINITION('Input outer spacer','Input outer spacer',#18111,
#18055);
#18063=PRODUCT_DEFINITION('Input bearing cap','Input bearing cap',#18112,
#18055);
#18064=PRODUCT_DEFINITION('Input bearing cap (1)','Input bearing cap (1)',
#18113,#18055);
#18065=PRODUCT_DEFINITION('Sliding bearing block',
'Sliding bearing block',#18114,#18055);
#18066=PRODUCT_DEFINITION('M4 clamp nut','M4 clamp nut',#18115,#18055);
#18067=PRODUCT_DEFINITION('M4 clamp nut (1)','M4 clamp nut (1)',#18116,#18055);
#18068=PRODUCT_DEFINITION('M4 clamp nut (2)','M4 clamp nut (2)',#18117,#18055);
#18069=PRODUCT_DEFINITION('M4 clamp nut (3)','M4 clamp nut (3)',#18118,#18055);
#18070=PRODUCT_DEFINITION('Output outer spacer','Output outer spacer',#18119,
#18055);
#18071=PRODUCT_DEFINITION('Output bearing cap','Output bearing cap',#18120,
#18055);
#18072=PRODUCT_DEFINITION('Output bearing cap (1)',
'Output bearing cap (1)',#18121,#18055);
#18073=PRODUCT_DEFINITION('Timing belt backing envelope',
'Timing belt backing envelope',#18122,#18055);
#18074=PRODUCT_DEFINITION('Sealed Ball Bearing - 10 x 30 x 9 mm',
'Sealed Ball Bearing - 10 x 30 x 9 mm',#18123,#18055);
#18075=PRODUCT_DEFINITION('Inner ring','Inner ring',#18124,#18055);
#18076=PRODUCT_DEFINITION('Outer ring','Outer ring',#18125,#18055);
#18077=PRODUCT_DEFINITION('Balls','Balls',#18126,#18055);
#18078=PRODUCT_DEFINITION('Cage','Cage',#18127,#18055);
#18079=PRODUCT_DEFINITION('Seals 2RS','Seals 2RS',#18128,#18055);
#18080=PRODUCT_DEFINITION('M4x30 mounting screw','M4x30 mounting screw',
#18129,#18055);
#18081=PRODUCT_DEFINITION('Sealed Ball Bearing - 12 x 32 x 10 mm',
'Sealed Ball Bearing - 12 x 32 x 10 mm',#18130,#18055);
#18082=PRODUCT_DEFINITION('Inner ring (1)','Inner ring (1)',#18131,#18055);
#18083=PRODUCT_DEFINITION('Outer ring (1)','Outer ring (1)',#18132,#18055);
#18084=PRODUCT_DEFINITION('Balls (1)','Balls (1)',#18133,#18055);
#18085=PRODUCT_DEFINITION('Cage (1)','Cage (1)',#18134,#18055);
#18086=PRODUCT_DEFINITION('Seals 2RS (1)','Seals 2RS (1)',#18135,#18055);
#18087=PRODUCT_DEFINITION('M4x10 Cap Screw','M4x10 Cap Screw',#18136,#18055);
#18088=PRODUCT_DEFINITION('Input pulley and shaft',
'Input pulley and shaft',#18137,#18055);
#18089=PRODUCT_DEFINITION('Input shaft','Input shaft',#18138,#18055);
#18090=PRODUCT_DEFINITION('Input inner spacer','Input inner spacer',#18139,
#18055);
#18091=PRODUCT_DEFINITION('Input inner sleeve','Input inner sleeve',#18140,
#18055);
#18092=PRODUCT_DEFINITION('Input M3 set screw','Input M3 set screw',#18141,
#18055);
#18093=PRODUCT_DEFINITION('Input M3 set screw (1)',
'Input M3 set screw (1)',#18142,#18055);
#18094=PRODUCT_DEFINITION('Input end keeper','Input end keeper',#18143,
#18055);
#18095=PRODUCT_DEFINITION(
'Timing Pulley - 2 mm Pitch, 20 Teeth, 8 mm Bore',
'Timing Pulley - 2 mm Pitch, 20 Teeth, 8 mm Bore',#18144,#18055);
#18096=PRODUCT_DEFINITION('Output pulley and shaft',
'Output pulley and shaft',#18145,#18055);
#18097=PRODUCT_DEFINITION('Output shaft','Output shaft',#18146,#18055);
#18098=PRODUCT_DEFINITION('Output inner spacer','Output inner spacer',#18147,
#18055);
#18099=PRODUCT_DEFINITION('Output inner sleeve','Output inner sleeve',#18148,
#18055);
#18100=PRODUCT_DEFINITION('Output M3 set screw','Output M3 set screw',#18149,
#18055);
#18101=PRODUCT_DEFINITION('Output M3 set screw (1)',
'Output M3 set screw (1)',#18150,#18055);
#18102=PRODUCT_DEFINITION('Output end keeper','Output end keeper',#18151,
#18055);
#18103=PRODUCT_DEFINITION(
'Timing Pulley - 2 mm Pitch, 40 Teeth, 12 mm Bore',
'Timing Pulley - 2 mm Pitch, 40 Teeth, 12 mm Bore',#18152,#18055);
#18104=PRODUCT_DEFINITION('Cap Screw - M4x16','Cap Screw - M4x16',#18153,
#18055);
#18105=PRODUCT_DEFINITION_FORMATION('',$,#18206);
#18106=PRODUCT_DEFINITION_FORMATION('',$,#18207);
#18107=PRODUCT_DEFINITION_FORMATION('',$,#18208);
#18108=PRODUCT_DEFINITION_FORMATION('',$,#18209);
#18109=PRODUCT_DEFINITION_FORMATION('',$,#18210);
#18110=PRODUCT_DEFINITION_FORMATION('',$,#18211);
#18111=PRODUCT_DEFINITION_FORMATION('',$,#18212);
#18112=PRODUCT_DEFINITION_FORMATION('',$,#18213);
#18113=PRODUCT_DEFINITION_FORMATION('',$,#18214);
#18114=PRODUCT_DEFINITION_FORMATION('',$,#18215);
#18115=PRODUCT_DEFINITION_FORMATION('',$,#18216);
#18116=PRODUCT_DEFINITION_FORMATION('',$,#18217);
#18117=PRODUCT_DEFINITION_FORMATION('',$,#18218);
#18118=PRODUCT_DEFINITION_FORMATION('',$,#18219);
#18119=PRODUCT_DEFINITION_FORMATION('',$,#18220);
#18120=PRODUCT_DEFINITION_FORMATION('',$,#18221);
#18121=PRODUCT_DEFINITION_FORMATION('',$,#18222);
#18122=PRODUCT_DEFINITION_FORMATION('',$,#18223);
#18123=PRODUCT_DEFINITION_FORMATION('',$,#18224);
#18124=PRODUCT_DEFINITION_FORMATION('',$,#18225);
#18125=PRODUCT_DEFINITION_FORMATION('',$,#18226);
#18126=PRODUCT_DEFINITION_FORMATION('',$,#18227);
#18127=PRODUCT_DEFINITION_FORMATION('',$,#18228);
#18128=PRODUCT_DEFINITION_FORMATION('',$,#18229);
#18129=PRODUCT_DEFINITION_FORMATION('',$,#18230);
#18130=PRODUCT_DEFINITION_FORMATION('',$,#18231);
#18131=PRODUCT_DEFINITION_FORMATION('',$,#18232);
#18132=PRODUCT_DEFINITION_FORMATION('',$,#18233);
#18133=PRODUCT_DEFINITION_FORMATION('',$,#18234);
#18134=PRODUCT_DEFINITION_FORMATION('',$,#18235);
#18135=PRODUCT_DEFINITION_FORMATION('',$,#18236);
#18136=PRODUCT_DEFINITION_FORMATION('',$,#18237);
#18137=PRODUCT_DEFINITION_FORMATION('',$,#18238);
#18138=PRODUCT_DEFINITION_FORMATION('',$,#18239);
#18139=PRODUCT_DEFINITION_FORMATION('',$,#18240);
#18140=PRODUCT_DEFINITION_FORMATION('',$,#18241);
#18141=PRODUCT_DEFINITION_FORMATION('',$,#18242);
#18142=PRODUCT_DEFINITION_FORMATION('',$,#18243);
#18143=PRODUCT_DEFINITION_FORMATION('',$,#18244);
#18144=PRODUCT_DEFINITION_FORMATION('',$,#18245);
#18145=PRODUCT_DEFINITION_FORMATION('',$,#18246);
#18146=PRODUCT_DEFINITION_FORMATION('',$,#18247);
#18147=PRODUCT_DEFINITION_FORMATION('',$,#18248);
#18148=PRODUCT_DEFINITION_FORMATION('',$,#18249);
#18149=PRODUCT_DEFINITION_FORMATION('',$,#18250);
#18150=PRODUCT_DEFINITION_FORMATION('',$,#18251);
#18151=PRODUCT_DEFINITION_FORMATION('',$,#18252);
#18152=PRODUCT_DEFINITION_FORMATION('',$,#18253);
#18153=PRODUCT_DEFINITION_FORMATION('',$,#18254);
#18154=PRODUCT_RELATED_PRODUCT_CATEGORY('PAT-104','PAT-104',(#18206));
#18155=PRODUCT_RELATED_PRODUCT_CATEGORY(
'Bearing base and belt envelope','Bearing base and belt envelope',(#18207));
#18156=PRODUCT_RELATED_PRODUCT_CATEGORY('Base','Base',(#18208));
#18157=PRODUCT_RELATED_PRODUCT_CATEGORY('Foot','Foot',(#18209));
#18158=PRODUCT_RELATED_PRODUCT_CATEGORY('Foot (1)','Foot (1)',(#18210));
#18159=PRODUCT_RELATED_PRODUCT_CATEGORY('Fixed bearing block',
'Fixed bearing block',(#18211));
#18160=PRODUCT_RELATED_PRODUCT_CATEGORY('Input outer spacer',
'Input outer spacer',(#18212));
#18161=PRODUCT_RELATED_PRODUCT_CATEGORY('Input bearing cap',
'Input bearing cap',(#18213));
#18162=PRODUCT_RELATED_PRODUCT_CATEGORY('Input bearing cap (1)',
'Input bearing cap (1)',(#18214));
#18163=PRODUCT_RELATED_PRODUCT_CATEGORY('Sliding bearing block',
'Sliding bearing block',(#18215));
#18164=PRODUCT_RELATED_PRODUCT_CATEGORY('M4 clamp nut','M4 clamp nut',(#18216));
#18165=PRODUCT_RELATED_PRODUCT_CATEGORY('M4 clamp nut (1)',
'M4 clamp nut (1)',(#18217));
#18166=PRODUCT_RELATED_PRODUCT_CATEGORY('M4 clamp nut (2)',
'M4 clamp nut (2)',(#18218));
#18167=PRODUCT_RELATED_PRODUCT_CATEGORY('M4 clamp nut (3)',
'M4 clamp nut (3)',(#18219));
#18168=PRODUCT_RELATED_PRODUCT_CATEGORY('Output outer spacer',
'Output outer spacer',(#18220));
#18169=PRODUCT_RELATED_PRODUCT_CATEGORY('Output bearing cap',
'Output bearing cap',(#18221));
#18170=PRODUCT_RELATED_PRODUCT_CATEGORY('Output bearing cap (1)',
'Output bearing cap (1)',(#18222));
#18171=PRODUCT_RELATED_PRODUCT_CATEGORY('Timing belt backing envelope',
'Timing belt backing envelope',(#18223));
#18172=PRODUCT_RELATED_PRODUCT_CATEGORY(
'Sealed Ball Bearing - 10 x 30 x 9 mm',
'Sealed Ball Bearing - 10 x 30 x 9 mm',(#18224));
#18173=PRODUCT_RELATED_PRODUCT_CATEGORY('Inner ring','Inner ring',(#18225));
#18174=PRODUCT_RELATED_PRODUCT_CATEGORY('Outer ring','Outer ring',(#18226));
#18175=PRODUCT_RELATED_PRODUCT_CATEGORY('Balls','Balls',(#18227));
#18176=PRODUCT_RELATED_PRODUCT_CATEGORY('Cage','Cage',(#18228));
#18177=PRODUCT_RELATED_PRODUCT_CATEGORY('Seals 2RS','Seals 2RS',(#18229));
#18178=PRODUCT_RELATED_PRODUCT_CATEGORY('M4x30 mounting screw',
'M4x30 mounting screw',(#18230));
#18179=PRODUCT_RELATED_PRODUCT_CATEGORY(
'Sealed Ball Bearing - 12 x 32 x 10 mm',
'Sealed Ball Bearing - 12 x 32 x 10 mm',(#18231));
#18180=PRODUCT_RELATED_PRODUCT_CATEGORY('Inner ring (1)',
'Inner ring (1)',(#18232));
#18181=PRODUCT_RELATED_PRODUCT_CATEGORY('Outer ring (1)',
'Outer ring (1)',(#18233));
#18182=PRODUCT_RELATED_PRODUCT_CATEGORY('Balls (1)','Balls (1)',(#18234));
#18183=PRODUCT_RELATED_PRODUCT_CATEGORY('Cage (1)','Cage (1)',(#18235));
#18184=PRODUCT_RELATED_PRODUCT_CATEGORY('Seals 2RS (1)','Seals 2RS (1)',
(#18236));
#18185=PRODUCT_RELATED_PRODUCT_CATEGORY('M4x10 Cap Screw',
'M4x10 Cap Screw',(#18237));
#18186=PRODUCT_RELATED_PRODUCT_CATEGORY('Input pulley and shaft',
'Input pulley and shaft',(#18238));
#18187=PRODUCT_RELATED_PRODUCT_CATEGORY('Input shaft','Input shaft',(#18239));
#18188=PRODUCT_RELATED_PRODUCT_CATEGORY('Input inner spacer',
'Input inner spacer',(#18240));
#18189=PRODUCT_RELATED_PRODUCT_CATEGORY('Input inner sleeve',
'Input inner sleeve',(#18241));
#18190=PRODUCT_RELATED_PRODUCT_CATEGORY('Input M3 set screw',
'Input M3 set screw',(#18242));
#18191=PRODUCT_RELATED_PRODUCT_CATEGORY('Input M3 set screw (1)',
'Input M3 set screw (1)',(#18243));
#18192=PRODUCT_RELATED_PRODUCT_CATEGORY('Input end keeper',
'Input end keeper',(#18244));
#18193=PRODUCT_RELATED_PRODUCT_CATEGORY(
'Timing Pulley - 2 mm Pitch, 20 Teeth, 8 mm Bore',
'Timing Pulley - 2 mm Pitch, 20 Teeth, 8 mm Bore',(#18245));
#18194=PRODUCT_RELATED_PRODUCT_CATEGORY('Output pulley and shaft',
'Output pulley and shaft',(#18246));
#18195=PRODUCT_RELATED_PRODUCT_CATEGORY('Output shaft','Output shaft',(#18247));
#18196=PRODUCT_RELATED_PRODUCT_CATEGORY('Output inner spacer',
'Output inner spacer',(#18248));
#18197=PRODUCT_RELATED_PRODUCT_CATEGORY('Output inner sleeve',
'Output inner sleeve',(#18249));
#18198=PRODUCT_RELATED_PRODUCT_CATEGORY('Output M3 set screw',
'Output M3 set screw',(#18250));
#18199=PRODUCT_RELATED_PRODUCT_CATEGORY('Output M3 set screw (1)',
'Output M3 set screw (1)',(#18251));
#18200=PRODUCT_RELATED_PRODUCT_CATEGORY('Output end keeper',
'Output end keeper',(#18252));
#18201=PRODUCT_RELATED_PRODUCT_CATEGORY(
'Timing Pulley - 2 mm Pitch, 40 Teeth, 12 mm Bore',
'Timing Pulley - 2 mm Pitch, 40 Teeth, 12 mm Bore',(#18253));
#18202=PRODUCT_RELATED_PRODUCT_CATEGORY('Cap Screw - M4x16',
'Cap Screw - M4x16',(#18254));
#18203=APPLICATION_PROTOCOL_DEFINITION('international standard',
'automotive_design',2009,#18204);
#18204=APPLICATION_CONTEXT(
'Core Data for Automotive Mechanical Design Process');
#18205=PRODUCT_CONTEXT('part definition',#18204,'mechanical');
#18206=PRODUCT('PAT-104',
'PAT-104','PAT-104',(#18205));
#18207=PRODUCT('Bearing base and belt envelope',
'Bearing base and belt envelope','Bearing base and belt envelope',(#18205));
#18208=PRODUCT('Base','Base','Base',(#18205));
#18209=PRODUCT('Foot','Foot','Foot',(#18205));
#18210=PRODUCT('Foot (1)','Foot (1)','Foot (1)',(#18205));
#18211=PRODUCT('Fixed bearing block','Fixed bearing block',
'Fixed bearing block',(#18205));
#18212=PRODUCT('Input outer spacer','Input outer spacer',
'Input outer spacer',(#18205));
#18213=PRODUCT('Input bearing cap','Input bearing cap',
'Input bearing cap',(#18205));
#18214=PRODUCT('Input bearing cap (1)','Input bearing cap (1)',
'Input bearing cap (1)',(#18205));
#18215=PRODUCT('Sliding bearing block','Sliding bearing block',
'Sliding bearing block',(#18205));
#18216=PRODUCT('M4 clamp nut','M4 clamp nut','M4 clamp nut',(#18205));
#18217=PRODUCT('M4 clamp nut (1)','M4 clamp nut (1)','M4 clamp nut (1)',(#18205));
#18218=PRODUCT('M4 clamp nut (2)','M4 clamp nut (2)','M4 clamp nut (2)',(#18205));
#18219=PRODUCT('M4 clamp nut (3)','M4 clamp nut (3)','M4 clamp nut (3)',(#18205));
#18220=PRODUCT('Output outer spacer','Output outer spacer',
'Output outer spacer',(#18205));
#18221=PRODUCT('Output bearing cap','Output bearing cap',
'Output bearing cap',(#18205));
#18222=PRODUCT('Output bearing cap (1)','Output bearing cap (1)',
'Output bearing cap (1)',(#18205));
#18223=PRODUCT('Timing belt backing envelope',
'Timing belt backing envelope','Timing belt backing envelope',(#18205));
#18224=PRODUCT('Sealed Ball Bearing - 10 x 30 x 9 mm',
'Sealed Ball Bearing - 10 x 30 x 9 mm',
'Sealed Ball Bearing - 10 x 30 x 9 mm',(#18205));
#18225=PRODUCT('Inner ring','Inner ring','Inner ring',(#18205));
#18226=PRODUCT('Outer ring','Outer ring','Outer ring',(#18205));
#18227=PRODUCT('Balls','Balls','Balls',(#18205));
#18228=PRODUCT('Cage','Cage','Cage',(#18205));
#18229=PRODUCT('Seals 2RS','Seals 2RS','Seals 2RS',(#18205));
#18230=PRODUCT('M4x30 mounting screw','M4x30 mounting screw',
'M4x30 mounting screw',(#18205));
#18231=PRODUCT('Sealed Ball Bearing - 12 x 32 x 10 mm',
'Sealed Ball Bearing - 12 x 32 x 10 mm',
'Sealed Ball Bearing - 12 x 32 x 10 mm',(#18205));
#18232=PRODUCT('Inner ring (1)','Inner ring (1)','Inner ring (1)',(#18205));
#18233=PRODUCT('Outer ring (1)','Outer ring (1)','Outer ring (1)',(#18205));
#18234=PRODUCT('Balls (1)','Balls (1)','Balls (1)',(#18205));
#18235=PRODUCT('Cage (1)','Cage (1)','Cage (1)',(#18205));
#18236=PRODUCT('Seals 2RS (1)','Seals 2RS (1)','Seals 2RS (1)',(#18205));
#18237=PRODUCT('M4x10 Cap Screw','M4x10 Cap Screw','M4x10 Cap Screw',(#18205));
#18238=PRODUCT('Input pulley and shaft','Input pulley and shaft',
'Input pulley and shaft',(#18205));
#18239=PRODUCT('Input shaft','Input shaft','Input shaft',(#18205));
#18240=PRODUCT('Input inner spacer','Input inner spacer',
'Input inner spacer',(#18205));
#18241=PRODUCT('Input inner sleeve','Input inner sleeve',
'Input inner sleeve',(#18205));
#18242=PRODUCT('Input M3 set screw','Input M3 set screw',
'Input M3 set screw',(#18205));
#18243=PRODUCT('Input M3 set screw (1)','Input M3 set screw (1)',
'Input M3 set screw (1)',(#18205));
#18244=PRODUCT('Input end keeper','Input end keeper','Input end keeper',
(#18205));
#18245=PRODUCT('Timing Pulley - 2 mm Pitch, 20 Teeth, 8 mm Bore',
'Timing Pulley - 2 mm Pitch, 20 Teeth, 8 mm Bore',
'Timing Pulley - 2 mm Pitch, 20 Teeth, 8 mm Bore',(#18205));
#18246=PRODUCT('Output pulley and shaft','Output pulley and shaft',
'Output pulley and shaft',(#18205));
#18247=PRODUCT('Output shaft','Output shaft','Output shaft',(#18205));
#18248=PRODUCT('Output inner spacer','Output inner spacer',
'Output inner spacer',(#18205));
#18249=PRODUCT('Output inner sleeve','Output inner sleeve',
'Output inner sleeve',(#18205));
#18250=PRODUCT('Output M3 set screw','Output M3 set screw',
'Output M3 set screw',(#18205));
#18251=PRODUCT('Output M3 set screw (1)','Output M3 set screw (1)',
'Output M3 set screw (1)',(#18205));
#18252=PRODUCT('Output end keeper','Output end keeper',
'Output end keeper',(#18205));
#18253=PRODUCT('Timing Pulley - 2 mm Pitch, 40 Teeth, 12 mm Bore',
'Timing Pulley - 2 mm Pitch, 40 Teeth, 12 mm Bore',
'Timing Pulley - 2 mm Pitch, 40 Teeth, 12 mm Bore',(#18205));
#18254=PRODUCT('Cap Screw - M4x16','Cap Screw - M4x16',
'Cap Screw - M4x16',(#18205));
#18255=PRESENTATION_STYLE_ASSIGNMENT((#18260));
#18256=PRESENTATION_STYLE_ASSIGNMENT((#18261));
#18257=PRESENTATION_STYLE_ASSIGNMENT((#18262));
#18258=PRESENTATION_STYLE_ASSIGNMENT((#18263));
#18259=PRESENTATION_STYLE_ASSIGNMENT((#18264));
#18260=SURFACE_STYLE_USAGE(.BOTH.,#18265);
#18261=SURFACE_STYLE_USAGE(.BOTH.,#18266);
#18262=SURFACE_STYLE_USAGE(.BOTH.,#18267);
#18263=SURFACE_STYLE_USAGE(.BOTH.,#18268);
#18264=SURFACE_STYLE_USAGE(.BOTH.,#18269);
#18265=SURFACE_SIDE_STYLE('',(#18270));
#18266=SURFACE_SIDE_STYLE('',(#18271));
#18267=SURFACE_SIDE_STYLE('',(#18272));
#18268=SURFACE_SIDE_STYLE('',(#18273));
#18269=SURFACE_SIDE_STYLE('',(#18274));
#18270=SURFACE_STYLE_FILL_AREA(#18275);
#18271=SURFACE_STYLE_FILL_AREA(#18276);
#18272=SURFACE_STYLE_FILL_AREA(#18277);
#18273=SURFACE_STYLE_FILL_AREA(#18278);
#18274=SURFACE_STYLE_FILL_AREA(#18279);
#18275=FILL_AREA_STYLE('Steel - Satin',(#18280));
#18276=FILL_AREA_STYLE('CAD Library Painted - Deep blue',(#18281));
#18277=FILL_AREA_STYLE('CAD Library Painted - Steel gray',(#18282));
#18278=FILL_AREA_STYLE('CAD Library Painted - Engineering blue',(#18283));
#18279=FILL_AREA_STYLE('CAD Library Painted - Graphite',(#18284));
#18280=FILL_AREA_STYLE_COLOUR('Steel - Satin',#18285);
#18281=FILL_AREA_STYLE_COLOUR('CAD Library Painted - Deep blue',#18286);
#18282=FILL_AREA_STYLE_COLOUR('CAD Library Painted - Steel gray',#18287);
#18283=FILL_AREA_STYLE_COLOUR('CAD Library Painted - Engineering blue',
#18288);
#18284=FILL_AREA_STYLE_COLOUR('CAD Library Painted - Graphite',#18289);
#18285=COLOUR_RGB('Steel - Satin',0.627450980392157,0.627450980392157,0.627450980392157);
#18286=COLOUR_RGB('CAD Library Painted - Deep blue',0.0784313725490196,
0.203921568627451,0.349019607843137);
#18287=COLOUR_RGB('CAD Library Painted - Steel gray',0.592156862745098,
0.631372549019608,0.67843137254902);
#18288=COLOUR_RGB('CAD Library Painted - Engineering blue',0.12156862745098,
0.356862745098039,0.6);
#18289=COLOUR_RGB('CAD Library Painted - Graphite',0.168627450980392,0.192156862745098,
0.231372549019608);
#18290=COLOUR_RGB('Dark Blue',0.08,0.2,0.34);
#18291=FILL_AREA_STYLE_COLOUR('',#18290);
#18292=FILL_AREA_STYLE('',(#18291));
#18293=SURFACE_STYLE_FILL_AREA(#18292);
#18294=SURFACE_SIDE_STYLE('',(#18293));
#18295=SURFACE_STYLE_USAGE(.BOTH.,#18294);
#18296=PRESENTATION_STYLE_ASSIGNMENT((#18295));
#18297=COLOUR_RGB('Light Blue',0.38,0.62,0.78);
#18298=FILL_AREA_STYLE_COLOUR('',#18297);
#18299=FILL_AREA_STYLE('',(#18298));
#18300=SURFACE_STYLE_FILL_AREA(#18299);
#18301=SURFACE_SIDE_STYLE('',(#18300));
#18302=SURFACE_STYLE_USAGE(.BOTH.,#18301);
#18303=PRESENTATION_STYLE_ASSIGNMENT((#18302));
#18304=COLOUR_RGB('Sky Blue',0.24,0.69,0.87);
#18305=FILL_AREA_STYLE_COLOUR('',#18304);
#18306=FILL_AREA_STYLE('',(#18305));
#18307=SURFACE_STYLE_FILL_AREA(#18306);
#18308=SURFACE_SIDE_STYLE('',(#18307));
#18309=SURFACE_STYLE_USAGE(.BOTH.,#18308);
#18310=PRESENTATION_STYLE_ASSIGNMENT((#18309));
#18311=COLOUR_RGB('Grey',0.48,0.52,0.57);
#18312=FILL_AREA_STYLE_COLOUR('',#18311);
#18313=FILL_AREA_STYLE('',(#18312));
#18314=SURFACE_STYLE_FILL_AREA(#18313);
#18315=SURFACE_SIDE_STYLE('',(#18314));
#18316=SURFACE_STYLE_USAGE(.BOTH.,#18315);
#18317=PRESENTATION_STYLE_ASSIGNMENT((#18316));
#18318=COLOUR_RGB('Black',0.12,0.14,0.17);
#18319=FILL_AREA_STYLE_COLOUR('',#18318);
#18320=FILL_AREA_STYLE('',(#18319));
#18321=SURFACE_STYLE_FILL_AREA(#18320);
#18322=SURFACE_SIDE_STYLE('',(#18321));
#18323=SURFACE_STYLE_USAGE(.BOTH.,#18322);
#18324=PRESENTATION_STYLE_ASSIGNMENT((#18323));
#18325=COLOUR_RGB('Off White',0.89,0.88,0.83);
#18326=FILL_AREA_STYLE_COLOUR('',#18325);
#18327=FILL_AREA_STYLE('',(#18326));
#18328=SURFACE_STYLE_FILL_AREA(#18327);
#18329=SURFACE_SIDE_STYLE('',(#18328));
#18330=SURFACE_STYLE_USAGE(.BOTH.,#18329);
#18331=PRESENTATION_STYLE_ASSIGNMENT((#18330));
ENDSEC;
END-ISO-10303-21;
